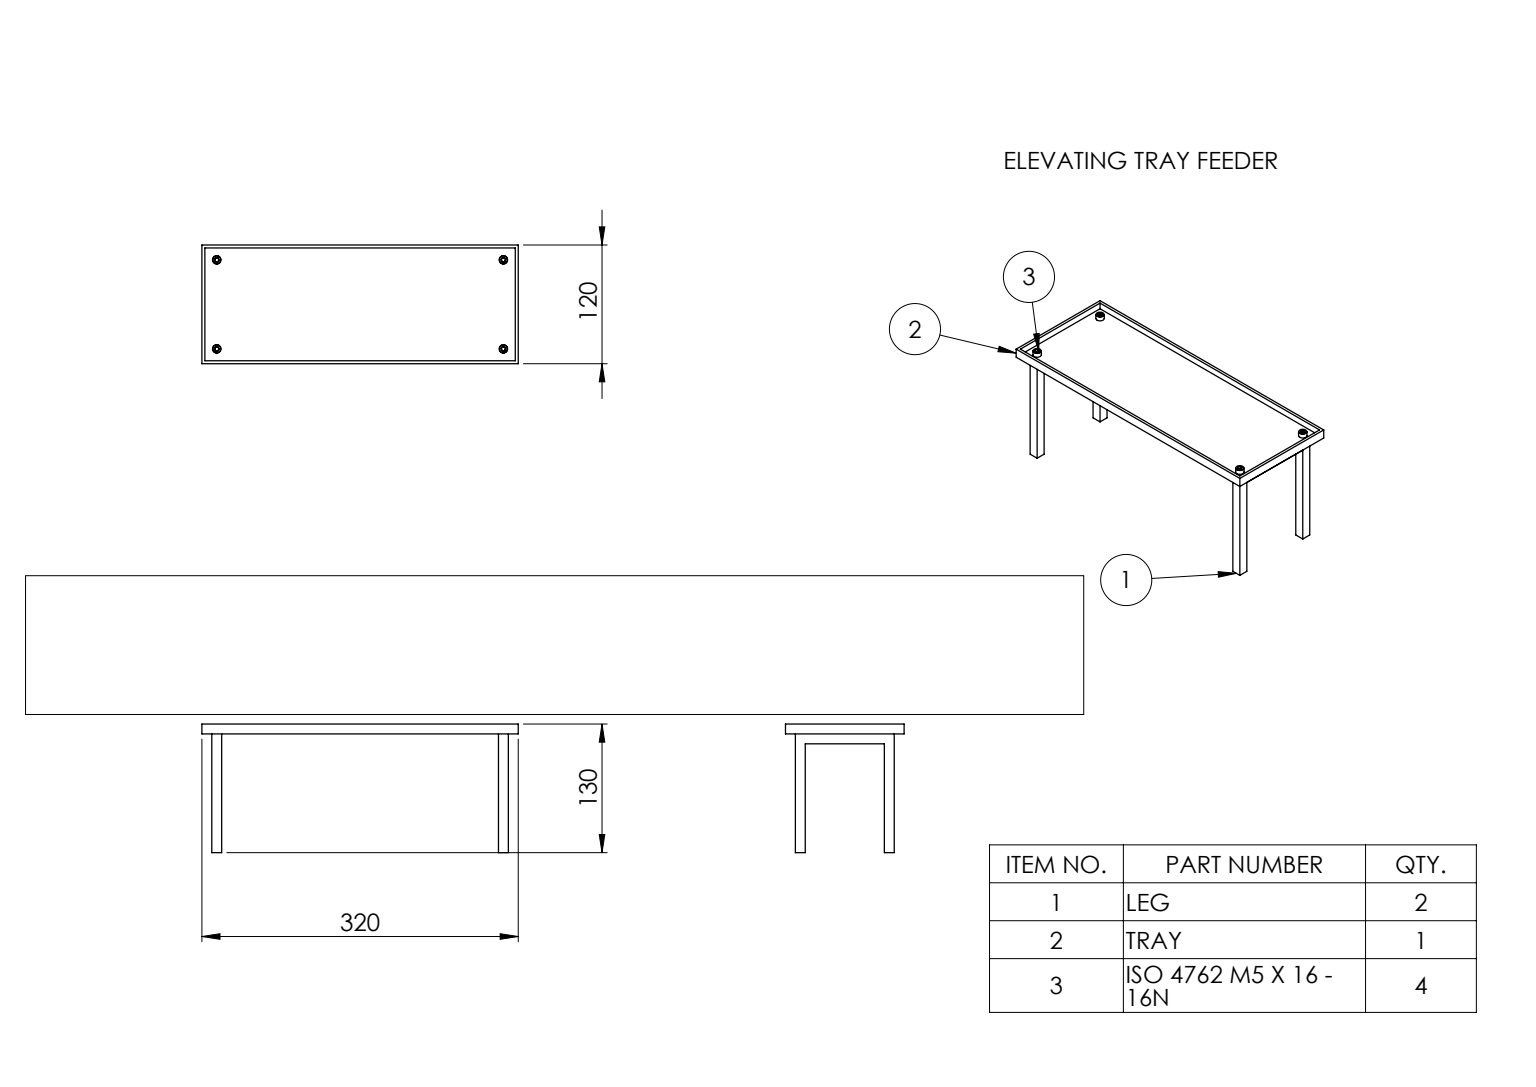
ISO-10303-21;
HEADER;
FILE_DESCRIPTION (('STEP AP214'),
    '1' );
FILE_NAME ('MAS-194',
    '2026-10-23T15:04:32',
    ( '' ),
    ( '' ),
    'SwSTEP 2.0',
    'SolidWorks 2026',
    '' );
FILE_SCHEMA (( 'AUTOMOTIVE_DESIGN' ));
ENDSEC;

DATA;
#1 = AXIS2_PLACEMENT_3D ( 'NONE', #713, #1643, #1457 ) ;
#2 = DIRECTION ( 'NONE',  ( 6.123233995736766036E-17, -1.000000000000000000, 0.000000000000000000 ) ) ;
#3 = AXIS2_PLACEMENT_3D ( 'NONE', #402, #1764, #2101 ) ;
#4 = VERTEX_POINT ( 'NONE', #2115 ) ;
#5 =( REPRESENTATION_RELATIONSHIP ('NONE','NONE', #367, #261 ) REPRESENTATION_RELATIONSHIP_WITH_TRANSFORMATION ( #2142 )SHAPE_REPRESENTATION_RELATIONSHIP( ) );
#6 = ORIENTED_EDGE ( 'NONE', *, *, #567, .F. ) ;
#7 = CARTESIAN_POINT ( 'NONE',  ( 145.0000000000000284, 2.993649167310367343, -47.64999999999998437 ) ) ;
#8 = PLANE ( 'NONE',  #1813 ) ;
#9 = CARTESIAN_POINT ( 'NONE',  ( -145.0000000000000284, -15.00000000000003197, 45.00000000000000000 ) ) ;
#10 = EDGE_CURVE ( 'NONE', #1293, #705, #989, .T. ) ;
#11 = DIRECTION ( 'NONE',  ( 0.000000000000000000, 0.5000000000000009992, 0.8660254037844380415 ) ) ;
#12 = CIRCLE ( 'NONE', #33, 2.500000000000002220 ) ;
#13 = EDGE_CURVE ( 'NONE', #1816, #847, #1494, .T. ) ;
#14 = ORIENTED_EDGE ( 'NONE', *, *, #1898, .T. ) ;
#15 = FACE_OUTER_BOUND ( 'NONE', #510, .T. ) ;
#16 = DIRECTION ( 'NONE',  ( -1.000000000000000000, 0.000000000000000000, 0.000000000000000000 ) ) ;
#17 = DIRECTION ( 'NONE',  ( 1.000000000000000000, 0.000000000000000000, 0.000000000000000000 ) ) ;
#18 = CIRCLE ( 'NONE', #321, 2.700000000000001066 ) ;
#19 = ORIENTED_EDGE ( 'NONE', *, *, #1395, .T. ) ;
#20 = DIRECTION ( 'NONE',  ( 0.000000000000000000, 0.000000000000000000, 1.000000000000000000 ) ) ;
#21 = CARTESIAN_POINT ( 'NONE',  ( 157.0000000000000000, 10.00000000000000000, 3.631354476378115974E-14 ) ) ;
#22 = FILL_AREA_STYLE ('',( #1265 ) ) ;
#23 = VECTOR ( 'NONE', #1974, 1000.000000000000000 ) ;
#24 = ORIENTED_EDGE ( 'NONE', *, *, #1544, .T. ) ;
#25 = CARTESIAN_POINT ( 'NONE',  ( -145.0000000000000284, 3.000000000000000000, -45.00000000000000000 ) ) ;
#26 = DIRECTION ( 'NONE',  ( -0.000000000000000000, 1.000000000000000000, -0.000000000000000000 ) ) ;
#27 = CYLINDRICAL_SURFACE ( 'NONE', #1694, 2.649999999999985700 ) ;
#28 = DIRECTION ( 'NONE',  ( 0.000000000000000000, -0.5000000000000009992, -0.8660254037844380415 ) ) ;
#29 = DIRECTION ( 'NONE',  ( -0.000000000000000000, -0.000000000000000000, -1.000000000000000000 ) ) ;
#30 = AXIS2_PLACEMENT_3D ( 'NONE', #971, #1660, #79 ) ;
#31 = CIRCLE ( 'NONE', #984, 2.649999999999985700 ) ;
#32 = EDGE_LOOP ( 'NONE', ( #1024, #985, #1536, #1885 ) ) ;
#33 = AXIS2_PLACEMENT_3D ( 'NONE', #1749, #1441, #229 ) ;
#34 = VECTOR ( 'NONE', #1991, 1000.000000000000000 ) ;
#35 = ORIENTED_EDGE ( 'NONE', *, *, #686, .F. ) ;
#36 = CYLINDRICAL_SURFACE ( 'NONE', #640, 2.649999999999985700 ) ;
#37 = CARTESIAN_POINT ( 'NONE',  ( 2.500000000000000000, 2.357898499370431722, -2.818925648462311528E-15 ) ) ;
#38 = SHAPE_REPRESENTATION ( 'leg', ( #30 ), #544 ) ;
#39 = DIRECTION ( 'NONE',  ( -6.123233995736766036E-17, 1.000000000000000000, -0.000000000000000000 ) ) ;
#40 = EDGE_CURVE ( 'NONE', #1625, #1348, #636, .T. ) ;
#41 = LINE ( 'NONE', #2054, #907 ) ;
#42 = PRODUCT_RELATED_PRODUCT_CATEGORY ( 'part', '', ( #72 ) ) ;
#43 = CARTESIAN_POINT ( 'NONE',  ( -150.0000000000000000, 0.000000000000000000, 50.00000000000000000 ) ) ;
#44 = VERTEX_POINT ( 'NONE', #1009 ) ;
#45 = ORIENTED_EDGE ( 'NONE', *, *, #1333, .T. ) ;
#46 = CARTESIAN_POINT ( 'NONE',  ( 160.0000000000000000, 0.000000000000000000, -60.00000000000000000 ) ) ;
#47 = CARTESIAN_POINT ( 'NONE',  ( 160.0000000000000000, 10.00000000000000000, -60.00000000000000000 ) ) ;
#48 = PLANE ( 'NONE',  #876 ) ;
#49 = ORIENTED_EDGE ( 'NONE', *, *, #111, .T. ) ;
#50 = DIRECTION ( 'NONE',  ( -0.000000000000000000, 1.000000000000000000, -0.000000000000000000 ) ) ;
#51 = AXIS2_PLACEMENT_3D ( 'NONE', #1269, #57, #1759 ) ;
#52 = CARTESIAN_POINT ( 'NONE',  ( -145.0000000000000284, -15.00000000000003197, -45.00000000000000000 ) ) ;
#53 = EDGE_CURVE ( 'NONE', #738, #333, #1664, .T. ) ;
#54 = ORIENTED_EDGE ( 'NONE', *, *, #1804, .F. ) ;
#55 = EDGE_CURVE ( 'NONE', #1358, #1353, #1429, .T. ) ;
#56 = ORIENTED_EDGE ( 'NONE', *, *, #696, .T. ) ;
#57 = DIRECTION ( 'NONE',  ( 6.123233995736766036E-17, -1.000000000000000000, 0.000000000000000000 ) ) ;
#58 = CARTESIAN_POINT ( 'NONE',  ( 0.000000000000000000, -1.178949249685214307, 2.042000000000001592 ) ) ;
#59 = DIRECTION ( 'NONE',  ( -0.000000000000000000, -1.000000000000000000, -0.000000000000000000 ) ) ;
#60 = VERTEX_POINT ( 'NONE', #817 ) ;
#61 = CIRCLE ( 'NONE', #2078, 2.500000000000002220 ) ;
#62 = DIRECTION ( 'NONE',  ( -0.000000000000000000, 0.000000000000000000, -1.000000000000000000 ) ) ;
#63 = LINE ( 'NONE', #106, #788 ) ;
#64 = ADVANCED_FACE ( 'NONE', ( #2182 ), #1857, .F. ) ;
#65 = VERTEX_POINT ( 'NONE', #648 ) ;
#66 = ADVANCED_FACE ( 'NONE', ( #1330, #2016 ), #1163, .F. ) ;
#67 = AXIS2_PLACEMENT_3D ( 'NONE', #1690, #1835, #1322 ) ;
#68 = ORIENTED_EDGE ( 'NONE', *, *, #53, .F. ) ;
#69 = DIRECTION ( 'NONE',  ( -1.000000000000000000, 0.000000000000000000, -0.000000000000000000 ) ) ;
#70 = LINE ( 'NONE', #2132, #1985 ) ;
#71 = AXIS2_PLACEMENT_3D ( 'NONE', #2013, #995, #1317 ) ;
#72 = PRODUCT ( 'leg', 'leg', '', ( #943 ) ) ;
#74 = ORIENTED_EDGE ( 'NONE', *, *, #1134, .T. ) ;
#73 = CARTESIAN_POINT ( 'NONE',  ( 145.0000000000000284, 2.993649167310367343, -45.00000000000000000 ) ) ;
#75 = CARTESIAN_POINT ( 'NONE',  ( 2.500000000000000000, 1.178949249685212974, -2.042000000000001148 ) ) ;
#76 = DIRECTION ( 'NONE',  ( 0.000000000000000000, 0.000000000000000000, 1.000000000000000000 ) ) ;
#77 = DIRECTION ( 'NONE',  ( 0.000000000000000000, 0.000000000000000000, -1.000000000000000000 ) ) ;
#78 = APPLICATION_PROTOCOL_DEFINITION ( 'draft international standard', 'automotive_design', 1998, #320 ) ;
#79 = DIRECTION ( 'NONE',  ( 1.000000000000000000, 0.000000000000000000, 0.000000000000000000 ) ) ;
#80 = VERTEX_POINT ( 'NONE', #828 ) ;
#81 = ORIENTED_EDGE ( 'NONE', *, *, #373, .T. ) ;
#82 = FACE_OUTER_BOUND ( 'NONE', #1924, .T. ) ;
#83 = FACE_OUTER_BOUND ( 'NONE', #1993, .T. ) ;
#84 = ORIENTED_EDGE ( 'NONE', *, *, #604, .T. ) ;
#86 = ORIENTED_EDGE ( 'NONE', *, *, #306, .T. ) ;
#85 = DIRECTION ( 'NONE',  ( 1.000000000000000000, 0.000000000000000000, 0.000000000000000000 ) ) ;
#87 = FACE_OUTER_BOUND ( 'NONE', #1431, .T. ) ;
#88 = VECTOR ( 'NONE', #539, 1000.000000000000000 ) ;
#89 = DIRECTION ( 'NONE',  ( -0.000000000000000000, 1.000000000000000000, -0.000000000000000000 ) ) ;
#90 = CARTESIAN_POINT ( 'NONE',  ( -157.0000000000000284, 10.00000000000000000, 57.00000000000000711 ) ) ;
#91 = VECTOR ( 'NONE', #730, 1000.000000000000114 ) ;
#92 = APPLICATION_PROTOCOL_DEFINITION ( 'draft international standard', 'automotive_design', 1998, #1085 ) ;
#93 =( LENGTH_UNIT ( ) NAMED_UNIT ( * ) SI_UNIT ( .MILLI., .METRE. ) );
#94 = VERTEX_POINT ( 'NONE', #1687 ) ;
#95 = EDGE_LOOP ( 'NONE', ( #1914, #1029, #1402 ) ) ;
#96 =( LENGTH_UNIT ( ) NAMED_UNIT ( * ) SI_UNIT ( .MILLI., .METRE. ) );
#97 = EDGE_LOOP ( 'NONE', ( #511, #45, #1713, #1611, #2168, #1515, #1183, #1829 ) ) ;
#98 = AXIS2_PLACEMENT_3D ( 'NONE', #2176, #427, #1287 ) ;
#100 = ORIENTED_EDGE ( 'NONE', *, *, #520, .T. ) ;
#99 = DIRECTION ( 'NONE',  ( 0.000000000000000000, 0.000000000000000000, 1.000000000000000000 ) ) ;
#101 = EDGE_CURVE ( 'NONE', #1631, #537, #2026, .T. ) ;
#102 = CARTESIAN_POINT ( 'NONE',  ( -160.0000000000000000, 10.00000000000000000, -56.99999999999997868 ) ) ;
#103 = AXIS2_PLACEMENT_3D ( 'NONE', #1867, #1367, #311 ) ;
#104 = AXIS2_PLACEMENT_3D ( 'NONE', #52, #222, #918 ) ;
#105 = CARTESIAN_POINT ( 'NONE',  ( 2.500000000000000000, 0.000000000000000000, 0.000000000000000000 ) ) ;
#106 = CARTESIAN_POINT ( 'NONE',  ( -139.9999999999999716, 2.312964634635743056E-15, -50.00000000000000000 ) ) ;
#107 = APPLICATION_PROTOCOL_DEFINITION ( 'draft international standard', 'automotive_design', 1998, #888 ) ;
#108 = ORIENTED_EDGE ( 'NONE', *, *, #1169, .T. ) ;
#109 = PLANE ( 'NONE',  #1726 ) ;
#110 = ORIENTED_EDGE ( 'NONE', *, *, #318, .F. ) ;
#111 = EDGE_CURVE ( 'NONE', #1963, #60, #1752, .T. ) ;
#112 = CARTESIAN_POINT ( 'NONE',  ( -139.9999999999999716, 2.312964634635743056E-15, 50.00000000000000000 ) ) ;
#113 = AXIS2_PLACEMENT_3D ( 'NONE', #174, #1044, #1337 ) ;
#114 = DIRECTION ( 'NONE',  ( 1.000000000000000000, 0.000000000000000000, -4.336808689942017736E-17 ) ) ;
#115 = ADVANCED_FACE ( 'NONE', ( #2005 ), #793, .T. ) ;
#116 = ADVANCED_FACE ( 'NONE', ( #1527 ), #1518, .T. ) ;
#117 =( GEOMETRIC_REPRESENTATION_CONTEXT ( 3 ) GLOBAL_UNCERTAINTY_ASSIGNED_CONTEXT ( ( #842 ) ) GLOBAL_UNIT_ASSIGNED_CONTEXT ( ( #1606, #589, #1445 ) ) REPRESENTATION_CONTEXT ( 'NONE', 'WORKASPACE' ) );
#118 = PRODUCT ( 'MAS-194', 'MAS-194', '', ( #1624 ) ) ;
#119 = CARTESIAN_POINT ( 'NONE',  ( -145.0000000000000284, 0.000000000000000000, 42.35000000000001563 ) ) ;
#120 = CARTESIAN_POINT ( 'NONE',  ( 156.9999999999999716, 3.000000000000000000, 57.00000000000000711 ) ) ;
#121 = EDGE_CURVE ( 'NONE', #1963, #166, #205, .T. ) ;
#122 = SHAPE_DEFINITION_REPRESENTATION ( #806, #367 ) ;
#123 = ORIENTED_EDGE ( 'NONE', *, *, #401, .T. ) ;
#124 = LINE ( 'NONE', #1842, #1158 ) ;
#125 = ORIENTED_EDGE ( 'NONE', *, *, #416, .T. ) ;
#126 = CARTESIAN_POINT ( 'NONE',  ( 21.00000000000000355, 0.000000000000000000, 0.000000000000000000 ) ) ;
#127 = LINE ( 'NONE', #2039, #1839 ) ;
#128 = DIRECTION ( 'NONE',  ( 1.000000000000000000, 0.000000000000000000, 0.000000000000000000 ) ) ;
#129 = AXIS2_PLACEMENT_3D ( 'NONE', #1889, #358, #1728 ) ;
#130 = DIRECTION ( 'NONE',  ( 0.000000000000000000, -1.000000000000000000, 0.000000000000000000 ) ) ;
#131 = FILL_AREA_STYLE_COLOUR ( '', #721 ) ;
#132 = ADVANCED_FACE ( 'NONE', ( #2209 ), #2220, .F. ) ;
#133 = ORIENTED_EDGE ( 'NONE', *, *, #586, .T. ) ;
#134 = DIRECTION ( 'NONE',  ( 2.312964634635742957E-16, -1.000000000000000000, 0.000000000000000000 ) ) ;
#135 = EDGE_CURVE ( 'NONE', #1670, #1316, #2046, .T. ) ;
#136 = ORIENTED_EDGE ( 'NONE', *, *, #518, .T. ) ;
#137 = CARTESIAN_POINT ( 'NONE',  ( 145.0000000000000284, 3.000000000000002665, -45.00000000000000000 ) ) ;
#138 = DIRECTION ( 'NONE',  ( 1.000000000000000000, 0.000000000000000000, 0.000000000000000000 ) ) ;
#139 = CIRCLE ( 'NONE', #605, 2.500000000000000444 ) ;
#140 = EDGE_LOOP ( 'NONE', ( #2012, #1805, #2066, #1757, #813 ) ) ;
#141 = DIRECTION ( 'NONE',  ( 0.000000000000000000, 0.000000000000000000, -1.000000000000000000 ) ) ;
#142 = DIRECTION ( 'NONE',  ( 0.000000000000000000, 0.000000000000000000, -1.000000000000000000 ) ) ;
#143 = SURFACE_SIDE_STYLE ('',( #858 ) ) ;
#144 = EDGE_CURVE ( 'NONE', #1505, #145, #1507, .T. ) ;
#145 = VERTEX_POINT ( 'NONE', #489 ) ;
#146 = ADVANCED_FACE ( 'NONE', ( #978 ), #2193, .F. ) ;
#147 = DIRECTION ( 'NONE',  ( -1.000000000000000000, 0.000000000000000000, -0.000000000000000000 ) ) ;
#148 = ORIENTED_EDGE ( 'NONE', *, *, #1970, .F. ) ;
#149 = CARTESIAN_POINT ( 'NONE',  ( 0.2500000000000002220, 0.000000000000000000, 0.000000000000000000 ) ) ;
#150 = CARTESIAN_POINT ( 'NONE',  ( 2.500000000000000000, 2.357898499370431722, -2.818925648462311528E-15 ) ) ;
#151 = ORIENTED_EDGE ( 'NONE', *, *, #1176, .T. ) ;
#152 = VECTOR ( 'NONE', #723, 1000.000000000000000 ) ;
#153 = DIRECTION ( 'NONE',  ( 0.000000000000000000, -1.000000000000000000, 0.000000000000000000 ) ) ;
#154 = FACE_OUTER_BOUND ( 'NONE', #1037, .T. ) ;
#155 = AXIS2_PLACEMENT_3D ( 'NONE', #797, #1356, #500 ) ;
#156 = AXIS2_PLACEMENT_3D ( 'NONE', #1101, #1761, #935 ) ;
#157 = ORIENTED_EDGE ( 'NONE', *, *, #401, .F. ) ;
#158 = ORIENTED_EDGE ( 'NONE', *, *, #281, .T. ) ;
#159 = DIRECTION ( 'NONE',  ( 0.000000000000000000, -1.000000000000000000, 0.000000000000000000 ) ) ;
#160 = CARTESIAN_POINT ( 'NONE',  ( -145.0000000000000284, 3.000000000000001776, -47.70000000000000284 ) ) ;
#161 = UNCERTAINTY_MEASURE_WITH_UNIT (LENGTH_MEASURE( 1.000000000000000082E-05 ), #96, 'distance_accuracy_value', 'NONE');
#162 = EDGE_LOOP ( 'NONE', ( #1939, #248, #188, #677 ) ) ;
#163 = CARTESIAN_POINT ( 'NONE',  ( -31.74999999999995737, 0.000000000000000000, 0.000000000000000000 ) ) ;
#164 = CARTESIAN_POINT ( 'NONE',  ( 5.200000000000002842, 0.000000000000000000, 2.500000000000000444 ) ) ;
#165 = EDGE_CURVE ( 'NONE', #314, #2053, #1896, .T. ) ;
#166 = VERTEX_POINT ( 'NONE', #1403 ) ;
#167 = ORIENTED_EDGE ( 'NONE', *, *, #1762, .T. ) ;
#168 = VECTOR ( 'NONE', #1538, 1000.000000000000000 ) ;
#169 = CYLINDRICAL_SURFACE ( 'NONE', #1242, 2.649999999999985700 ) ;
#170 = CARTESIAN_POINT ( 'NONE',  ( -157.0000000000000000, 10.00000000000000000, -3.631354476378115974E-14 ) ) ;
#171 = ADVANCED_FACE ( 'NONE', ( #512 ), #704, .T. ) ;
#172 = EDGE_LOOP ( 'NONE', ( #1456, #1524 ) ) ;
#173 = DIRECTION ( 'NONE',  ( -1.000000000000000000, 0.000000000000000000, 0.000000000000000000 ) ) ;
#174 = CARTESIAN_POINT ( 'NONE',  ( 0.000000000000000000, 0.000000000000000000, 0.000000000000000000 ) ) ;
#175 = CLOSED_SHELL ( 'NONE', ( #313, #917, #64, #1213, #1876, #1890, #1705, #1823, #1721, #1503, #2061, #116, #1440, #2153, #1530, #1941, #1489, #1042 ) ) ;
#176 = ORIENTED_EDGE ( 'NONE', *, *, #1772, .T. ) ;
#177 = AXIS2_PLACEMENT_3D ( 'NONE', #1608, #438, #449 ) ;
#178 = ORIENTED_EDGE ( 'NONE', *, *, #684, .F. ) ;
#179 = FACE_OUTER_BOUND ( 'NONE', #272, .T. ) ;
#180 = EDGE_CURVE ( 'NONE', #226, #627, #965, .T. ) ;
#181 = CARTESIAN_POINT ( 'NONE',  ( -160.0000000000000284, 0.000000000000000000, 60.00000000000001421 ) ) ;
#182 = AXIS2_PLACEMENT_3D ( 'NONE', #632, #455, #1006 ) ;
#183 = AXIS2_PLACEMENT_3D ( 'NONE', #2092, #526, #1052 ) ;
#184 = ADVANCED_FACE ( 'NONE', ( #1232 ), #388, .T. ) ;
#185 = DIRECTION ( 'NONE',  ( 0.000000000000000000, 0.000000000000000000, -1.000000000000000000 ) ) ;
#186 = EDGE_CURVE ( 'NONE', #1465, #166, #1054, .T. ) ;
#187 = AXIS2_PLACEMENT_3D ( 'NONE', #646, #1683, #147 ) ;
#188 = ORIENTED_EDGE ( 'NONE', *, *, #880, .T. ) ;
#189 = CARTESIAN_POINT ( 'NONE',  ( 5.200000000000002842, 0.000000000000000000, 0.000000000000000000 ) ) ;
#190 = DIRECTION ( 'NONE',  ( 0.000000000000000000, -0.4999999999999989453, 0.8660254037844391517 ) ) ;
#191 = CARTESIAN_POINT ( 'NONE',  ( -145.0000000000000284, -15.00000000000003197, 47.50000000000000000 ) ) ;
#192 = DIRECTION ( 'NONE',  ( -1.000000000000000000, -0.000000000000000000, -0.000000000000000000 ) ) ;
#193 = LINE ( 'NONE', #908, #1216 ) ;
#194 = CIRCLE ( 'NONE', #1276, 2.500000000000002220 ) ;
#195 = ORIENTED_EDGE ( 'NONE', *, *, #283, .T. ) ;
#196 = CARTESIAN_POINT ( 'NONE',  ( 2.500000000000000000, 1.178949249685212974, -2.042000000000001148 ) ) ;
#197 = EDGE_CURVE ( 'NONE', #1465, #610, #889, .T. ) ;
#198 = DIRECTION ( 'NONE',  ( -0.000000000000000000, 1.000000000000000000, -0.000000000000000000 ) ) ;
#199 = LINE ( 'NONE', #1861, #548 ) ;
#200 = CARTESIAN_POINT ( 'NONE',  ( 5.200000000000002842, 0.000000000000000000, 0.000000000000000000 ) ) ;
#201 = DIRECTION ( 'NONE',  ( -1.000000000000000000, -0.000000000000000000, -0.000000000000000000 ) ) ;
#202 = CARTESIAN_POINT ( 'NONE',  ( 145.0000000000000284, 3.000000000000001776, -47.70000000000000284 ) ) ;
#203 = AXIS2_PLACEMENT_3D ( 'NONE', #709, #130, #651 ) ;
#204 = ORIENTED_EDGE ( 'NONE', *, *, #1315, .F. ) ;
#205 = CIRCLE ( 'NONE', #1463, 2.649999999999985700 ) ;
#206 = ORIENTED_EDGE ( 'NONE', *, *, #1935, .T. ) ;
#207 = DIRECTION ( 'NONE',  ( 1.000000000000000000, 0.000000000000000000, 0.000000000000000000 ) ) ;
#208 = EDGE_CURVE ( 'NONE', #749, #899, #1717, .T. ) ;
#209 = DIRECTION ( 'NONE',  ( 0.000000000000000000, 0.000000000000000000, -1.000000000000000000 ) ) ;
#210 = CARTESIAN_POINT ( 'NONE',  ( -160.0000000000000000, 10.00000000000000000, -59.99999999999998579 ) ) ;
#211 = DIRECTION ( 'NONE',  ( 0.000000000000000000, 0.000000000000000000, -1.000000000000000000 ) ) ;
#212 = CARTESIAN_POINT ( 'NONE',  ( 2.500000000000000000, -2.357898499370432166, 3.035766082959412415E-15 ) ) ;
#213 = PRESENTATION_LAYER_ASSIGNMENT (  '', '', ( #1119 ) ) ;
#214 = EDGE_LOOP ( 'NONE', ( #762, #945, #1306, #1209 ) ) ;
#215 = PRESENTATION_LAYER_ASSIGNMENT (  '', '', ( #341 ) ) ;
#216 = VERTEX_POINT ( 'NONE', #7 ) ;
#217 = FACE_OUTER_BOUND ( 'NONE', #1185, .T. ) ;
#218 = CARTESIAN_POINT ( 'NONE',  ( 160.0000000000000000, 10.00000000000000000, -60.00000000000000000 ) ) ;
#219 = DIRECTION ( 'NONE',  ( 4.336808689942017736E-17, -0.000000000000000000, 1.000000000000000000 ) ) ;
#220 = VERTEX_POINT ( 'NONE', #2089 ) ;
#221 = FILL_AREA_STYLE_COLOUR ( '', #1658 ) ;
#222 = DIRECTION ( 'NONE',  ( -0.000000000000000000, 1.000000000000000000, -0.000000000000000000 ) ) ;
#223 = DIRECTION ( 'NONE',  ( -1.000000000000000000, -6.123233995736766036E-17, -0.000000000000000000 ) ) ;
#224 = EDGE_CURVE ( 'NONE', #575, #1831, #600, .T. ) ;
#225 = ORIENTED_EDGE ( 'NONE', *, *, #1492, .F. ) ;
#226 = VERTEX_POINT ( 'NONE', #357 ) ;
#227 = CIRCLE ( 'NONE', #385, 2.700000000000001066 ) ;
#228 = LINE ( 'NONE', #585, #1036 ) ;
#229 = DIRECTION ( 'NONE',  ( 0.000000000000000000, 0.000000000000000000, 1.000000000000000000 ) ) ;
#230 = CARTESIAN_POINT ( 'NONE',  ( -160.0000000000000284, 10.00000000000000000, 60.00000000000001421 ) ) ;
#231 = CARTESIAN_POINT ( 'NONE',  ( -2.471980953266949321E-15, 3.000000000000000000, -56.99999999999998579 ) ) ;
#232 = EDGE_CURVE ( 'NONE', #65, #2053, #1572, .T. ) ;
#233 = CIRCLE ( 'NONE', #866, 4.250000000000000000 ) ;
#234 = ORIENTED_EDGE ( 'NONE', *, *, #1075, .T. ) ;
#235 = ORIENTED_EDGE ( 'NONE', *, *, #197, .F. ) ;
#236 = CARTESIAN_POINT ( 'NONE',  ( 3.678949249685231848, 0.000000000000000000, 0.000000000000000000 ) ) ;
#237 = DIRECTION ( 'NONE',  ( -0.000000000000000000, -0.000000000000000000, -1.000000000000000000 ) ) ;
#238 = FACE_OUTER_BOUND ( 'NONE', #1600, .T. ) ;
#240 = VERTEX_POINT ( 'NONE', #1377 ) ;
#239 = CARTESIAN_POINT ( 'NONE',  ( 2.500000000000000000, 2.357898499370431722, -2.818925648462311528E-15 ) ) ;
#241 = PRESENTATION_STYLE_ASSIGNMENT (( #2112 ) ) ;
#242 = AXIS2_PLACEMENT_3D ( 'NONE', #919, #223, #2104 ) ;
#243 = DIRECTION ( 'NONE',  ( -1.000000000000000000, 0.000000000000000000, 4.336808689942017736E-17 ) ) ;
#244 = DIRECTION ( 'NONE',  ( -5.046468293750711010E-16, 1.000000000000000000, 0.000000000000000000 ) ) ;
#245 = CONTEXT_DEPENDENT_SHAPE_REPRESENTATION ( #1913, #2164 ) ;
#246 = ADVANCED_FACE ( 'NONE', ( #1385 ), #1674, .T. ) ;
#247 =( LENGTH_UNIT ( ) NAMED_UNIT ( * ) SI_UNIT ( .MILLI., .METRE. ) );
#248 = ORIENTED_EDGE ( 'NONE', *, *, #706, .T. ) ;
#249 = ORIENTED_EDGE ( 'NONE', *, *, #424, .F. ) ;
#250 = VECTOR ( 'NONE', #1166, 1000.000000000000000 ) ;
#251 = ORIENTED_EDGE ( 'NONE', *, *, #1272, .F. ) ;
#252 = DIRECTION ( 'NONE',  ( -0.000000000000000000, 1.000000000000000000, -0.000000000000000000 ) ) ;
#253 = CARTESIAN_POINT ( 'NONE',  ( -145.0000000000000284, 3.000000000000002665, 45.00000000000000000 ) ) ;
#254 = CIRCLE ( 'NONE', #3, 4.000000000000000000 ) ;
#255 = VECTOR ( 'NONE', #2191, 1000.000000000000000 ) ;
#256 = VERTEX_POINT ( 'NONE', #1555 ) ;
#257 = PRODUCT_DEFINITION_SHAPE ( 'NONE', 'NONE',  #2227 ) ;
#259 = ORIENTED_EDGE ( 'NONE', *, *, #781, .F. ) ;
#258 = DIRECTION ( 'NONE',  ( -0.000000000000000000, 1.000000000000000000, -0.000000000000000000 ) ) ;
#260 = DIRECTION ( 'NONE',  ( -1.000000000000000000, -6.123233995736766036E-17, -0.000000000000000000 ) ) ;
#261 = SHAPE_REPRESENTATION ( 'tray', ( #30 ), #1049 ) ;
#262 = DIRECTION ( 'NONE',  ( 0.000000000000000000, -1.000000000000000000, 0.000000000000000000 ) ) ;
#263 = LINE ( 'NONE', #90, #1184 ) ;
#264 = SURFACE_STYLE_USAGE ( .BOTH. , #1999 ) ;
#265 = ORIENTED_EDGE ( 'NONE', *, *, #1150, .F. ) ;
#266 = EDGE_CURVE ( 'NONE', #1421, #653, #1916, .T. ) ;
#267 = VERTEX_POINT ( 'NONE', #707 ) ;
#268 = DIRECTION ( 'NONE',  ( 0.000000000000000000, 0.000000000000000000, -1.000000000000000000 ) ) ;
#269 = CARTESIAN_POINT ( 'NONE',  ( -150.0000000000000000, 0.000000000000000000, -50.00000000000000000 ) ) ;
#270 = EDGE_LOOP ( 'NONE', ( #655, #206, #1374 ) ) ;
#272 = EDGE_LOOP ( 'NONE', ( #1135, #854, #1328, #1129 ) ) ;
#271 = LINE ( 'NONE', #1566, #1453 ) ;
#273 = CARTESIAN_POINT ( 'NONE',  ( 145.0000000000000284, 2.800000000000000266, -45.00000000000000000 ) ) ;
#274 = AXIS2_PLACEMENT_3D ( 'NONE', #873, #679, #190 ) ;
#275 = CARTESIAN_POINT ( 'NONE',  ( 0.000000000000000000, 0.000000000000000000, 50.00000000000000000 ) ) ;
#276 = FACE_OUTER_BOUND ( 'NONE', #1110, .T. ) ;
#277 = AXIS2_PLACEMENT_3D ( 'NONE', #538, #1561, #1211 ) ;
#278 = DIRECTION ( 'NONE',  ( 1.000000000000000000, 0.000000000000000000, 0.000000000000000000 ) ) ;
#279 = PRODUCT_DEFINITION_SHAPE ( 'NONE', 'NONE',  #1642 ) ;
#280 = ORIENTED_EDGE ( 'NONE', *, *, #988, .T. ) ;
#281 = EDGE_CURVE ( 'NONE', #240, #1735, #1638, .T. ) ;
#282 = ORIENTED_EDGE ( 'NONE', *, *, #559, .F. ) ;
#283 = EDGE_CURVE ( 'NONE', #1794, #1470, #1533, .T. ) ;
#284 = CARTESIAN_POINT ( 'NONE',  ( -145.0000000000000284, -15.00000000000003197, 42.49999999999999289 ) ) ;
#285 = ORIENTED_EDGE ( 'NONE', *, *, #1767, .T. ) ;
#286 = AXIS2_PLACEMENT_3D ( 'NONE', #1522, #857, #1497 ) ;
#287 = ADVANCED_FACE ( 'NONE', ( #15 ), #36, .F. ) ;
#288 = DIRECTION ( 'NONE',  ( 0.000000000000000000, -0.5000000000000013323, -0.8660254037844380415 ) ) ;
#289 = DIRECTION ( 'NONE',  ( 0.000000000000000000, 0.000000000000000000, 1.000000000000000000 ) ) ;
#290 = CLOSED_SHELL ( 'NONE', ( #1208, #1730, #801, #1062, #184, #534, #1347, #1500, #1560, #469, #1546, #374, #979, #115, #1267, #2103, #1607, #1259, #869, #1380, #531, #1775, #1016, #132, #451, #1373, #1562 ) ) ;
#291 = COLOUR_RGB ( '',0.8941176470588234615, 0.8941176470588234615, 0.8941176470588234615 ) ;
#292 = CARTESIAN_POINT ( 'NONE',  ( 0.000000000000000000, -2.357898499370432166, 3.035766082959412415E-15 ) ) ;
#293 = CARTESIAN_POINT ( 'NONE',  ( 2.500000000000000000, 1.178949249685217415, 2.041999999999998483 ) ) ;
#294 = ORIENTED_EDGE ( 'NONE', *, *, #359, .T. ) ;
#295 = DIRECTION ( 'NONE',  ( 0.000000000000000000, -0.5000000000000009992, -0.8660254037844380415 ) ) ;
#296 = ORIENTED_EDGE ( 'NONE', *, *, #1610, .F. ) ;
#297 =( GEOMETRIC_REPRESENTATION_CONTEXT ( 3 ) GLOBAL_UNCERTAINTY_ASSIGNED_CONTEXT ( ( #1869 ) ) GLOBAL_UNIT_ASSIGNED_CONTEXT ( ( #1381, #1558, #1182 ) ) REPRESENTATION_CONTEXT ( 'NONE', 'WORKASPACE' ) );
#298 = AXIS2_PLACEMENT_3D ( 'NONE', #2174, #1189, #2020 ) ;
#299 = DIRECTION ( 'NONE',  ( 0.000000000000000000, 0.5150380749100541555, 0.8571673007021122226 ) ) ;
#300 = AXIS2_PLACEMENT_3D ( 'NONE', #508, #495, #1703 ) ;
#301 = CARTESIAN_POINT ( 'NONE',  ( 2.500000000000000000, 0.000000000000000000, 0.000000000000000000 ) ) ;
#302 = AXIS2_PLACEMENT_3D ( 'NONE', #75, #1797, #1080 ) ;
#303 = CARTESIAN_POINT ( 'NONE',  ( 2.500000000000000000, 1.178949249685212974, -2.042000000000001148 ) ) ;
#304 = DIRECTION ( 'NONE',  ( -1.000000000000000000, -0.000000000000000000, -0.000000000000000000 ) ) ;
#305 = ADVANCED_FACE ( 'NONE', ( #1736 ), #169, .F. ) ;
#306 = EDGE_CURVE ( 'NONE', #4, #1672, #1360, .T. ) ;
#307 =( NAMED_UNIT ( * ) PLANE_ANGLE_UNIT ( ) SI_UNIT ( $, .RADIAN. ) );
#308 = ORIENTED_EDGE ( 'NONE', *, *, #734, .F. ) ;
#309 = CARTESIAN_POINT ( 'NONE',  ( -139.9999999999999716, -120.0000000000000142, 40.00000000000000000 ) ) ;
#310 = ORIENTED_EDGE ( 'NONE', *, *, #2133, .T. ) ;
#311 = DIRECTION ( 'NONE',  ( 0.000000000000000000, -1.000000000000000000, 0.000000000000000000 ) ) ;
#312 = CARTESIAN_POINT ( 'NONE',  ( 0.000000000000000000, 0.000000000000000000, 0.000000000000000000 ) ) ;
#313 = ADVANCED_FACE ( 'NONE', ( #1926 ), #1245, .F. ) ;
#314 = VERTEX_POINT ( 'NONE', #236 ) ;
#315 = DIRECTION ( 'NONE',  ( -6.123233995736766036E-17, 1.000000000000000000, -0.000000000000000000 ) ) ;
#316 = CIRCLE ( 'NONE', #1206, 2.500000000000000888 ) ;
#317 = CARTESIAN_POINT ( 'NONE',  ( -145.0000000000000284, 0.000000000000000000, -45.00000000000000000 ) ) ;
#318 = EDGE_CURVE ( 'NONE', #2053, #1816, #228, .T. ) ;
#319 = PRESENTATION_STYLE_ASSIGNMENT (( #1548 ) ) ;
#320 = APPLICATION_CONTEXT ( 'automotive_design' ) ;
#321 = AXIS2_PLACEMENT_3D ( 'NONE', #1424, #399, #1951 ) ;
#322 = ORIENTED_EDGE ( 'NONE', *, *, #1708, .F. ) ;
#323 = DIRECTION ( 'NONE',  ( -0.000000000000000000, 1.000000000000000000, -0.000000000000000000 ) ) ;
#324 = VERTEX_POINT ( 'NONE', #2098 ) ;
#325 = DIRECTION ( 'NONE',  ( -1.000000000000000000, -0.000000000000000000, -0.000000000000000000 ) ) ;
#326 = DIRECTION ( 'NONE',  ( 6.123233995736766036E-17, -1.000000000000000000, 0.000000000000000000 ) ) ;
#327 = AXIS2_PLACEMENT_3D ( 'NONE', #1511, #1026, #1679 ) ;
#328 = ORIENTED_EDGE ( 'NONE', *, *, #868, .F. ) ;
#329 = FACE_OUTER_BOUND ( 'NONE', #1684, .T. ) ;
#330 = DIRECTION ( 'NONE',  ( 2.312964634635742957E-16, 0.000000000000000000, -1.000000000000000000 ) ) ;
#331 = DIRECTION ( 'NONE',  ( 0.000000000000000000, 0.000000000000000000, 1.000000000000000000 ) ) ;
#332 = ORIENTED_EDGE ( 'NONE', *, *, #1547, .T. ) ;
#333 = VERTEX_POINT ( 'NONE', #561 ) ;
#334 = EDGE_CURVE ( 'NONE', #396, #60, #18, .T. ) ;
#335 = CARTESIAN_POINT ( 'NONE',  ( -139.9999999999999716, -120.0000000000000142, 40.00000000000000000 ) ) ;
#336 = MECHANICAL_DESIGN_GEOMETRIC_PRESENTATION_REPRESENTATION (  '', ( #1119 ), #1476 ) ;
#337 = ORIENTED_EDGE ( 'NONE', *, *, #2208, .F. ) ;
#338 = VECTOR ( 'NONE', #28, 1000.000000000000114 ) ;
#339 = CARTESIAN_POINT ( 'NONE',  ( -157.0000000000000284, 3.000000000000000000, 57.00000000000000711 ) ) ;
#340 = DIRECTION ( 'NONE',  ( -2.312964634635743450E-16, 1.000000000000000000, 0.000000000000000000 ) ) ;
#341=STYLED_ITEM('',(#2247),#969);
#342 = DIRECTION ( 'NONE',  ( -1.000000000000000000, 0.000000000000000000, 0.000000000000000000 ) ) ;
#343 = EDGE_LOOP ( 'NONE', ( #996, #736, #151, #176 ) ) ;
#344 = VERTEX_POINT ( 'NONE', #572 ) ;
#345 = ADVANCED_FACE ( 'NONE', ( #1256 ), #564, .T. ) ;
#346 = DIRECTION ( 'NONE',  ( 0.000000000000000000, 0.000000000000000000, 1.000000000000000000 ) ) ;
#347 = CARTESIAN_POINT ( 'NONE',  ( -139.9999999999999716, -120.0000000000000142, -40.00000000000000000 ) ) ;
#348 = UNCERTAINTY_MEASURE_WITH_UNIT (LENGTH_MEASURE( 1.000000000000000082E-05 ), #93, 'distance_accuracy_value', 'NONE');
#349 = EDGE_LOOP ( 'NONE', ( #249, #593, #1950, #1766 ) ) ;
#350 = DIRECTION ( 'NONE',  ( 1.000000000000000000, 0.000000000000000000, 0.000000000000000000 ) ) ;
#351 = EDGE_LOOP ( 'NONE', ( #436, #2147 ) ) ;
#352 = ADVANCED_FACE ( 'NONE', ( #217 ), #1742, .T. ) ;
#353 = VERTEX_POINT ( 'NONE', #46 ) ;
#354 = SHAPE_REPRESENTATION ( 'socket head cap screw_iso_ISO 4762 M5 x 16 - 16N', ( #30 ), #1018 ) ;
#355 = AXIS2_PLACEMENT_3D ( 'NONE', #1066, #872, #1906 ) ;
#356 = EDGE_CURVE ( 'NONE', #705, #671, #1769, .T. ) ;
#357 = CARTESIAN_POINT ( 'NONE',  ( 5.000000000000002665, 0.000000000000000000, -2.700000000000000622 ) ) ;
#358 = DIRECTION ( 'NONE',  ( 6.123233995736766036E-17, -1.000000000000000000, 0.000000000000000000 ) ) ;
#359 = EDGE_CURVE ( 'NONE', #738, #1430, #1432, .T. ) ;
#360 = CARTESIAN_POINT ( 'NONE',  ( 2.500000000000000000, 1.768423874527822459, -1.021000000000002794 ) ) ;
#361 = COLOUR_RGB ( '',1.000000000000000000, 0.9490196078431372140, 0.9098039215686274384 ) ;
#362 = CARTESIAN_POINT ( 'NONE',  ( 0.000000000000000000, 0.000000000000000000, 0.000000000000000000 ) ) ;
#363 = PRESENTATION_LAYER_ASSIGNMENT (  '', '', ( #1329 ) ) ;
#364 = ORIENTED_EDGE ( 'NONE', *, *, #1034, .F. ) ;
#365 = DIRECTION ( 'NONE',  ( 0.000000000000000000, 0.000000000000000000, -1.000000000000000000 ) ) ;
#366 = CARTESIAN_POINT ( 'NONE',  ( -145.0000000000000284, -16.50215154756893554, 45.00000000000000000 ) ) ;
#367 = SHAPE_REPRESENTATION ( 'MAS-194', ( #1338, #691, #113, #1944, #1262, #300, #874, #369 ), #476 ) ;
#368 = FACE_OUTER_BOUND ( 'NONE', #1880, .T. ) ;
#369 = AXIS2_PLACEMENT_3D ( 'NONE', #1523, #2216, #1191 ) ;
#370 = VECTOR ( 'NONE', #446, 1000.000000000000000 ) ;
#371 = DIRECTION ( 'NONE',  ( 0.000000000000000000, -0.5000000000000013323, -0.8660254037844380415 ) ) ;
#372 = VECTOR ( 'NONE', #803, 1000.000000000000000 ) ;
#373 = EDGE_CURVE ( 'NONE', #1909, #1887, #2134, .T. ) ;
#374 = ADVANCED_FACE ( 'NONE', ( #1128 ), #1994, .T. ) ;
#375 = EDGE_LOOP ( 'NONE', ( #1502, #922, #259, #2033 ) ) ;
#376 = LINE ( 'NONE', #347, #1059 ) ;
#377 = DIRECTION ( 'NONE',  ( 0.000000000000000000, -1.000000000000000000, 0.000000000000000000 ) ) ;
#378 = EDGE_CURVE ( 'NONE', #220, #830, #1795, .T. ) ;
#379 = EDGE_LOOP ( 'NONE', ( #1466, #491 ) ) ;
#380 = LINE ( 'NONE', #554, #722 ) ;
#381 = EDGE_CURVE ( 'NONE', #344, #473, #457, .T. ) ;
#382 = DIRECTION ( 'NONE',  ( 1.000000000000000000, 0.000000000000000000, 0.000000000000000000 ) ) ;
#383 = DIRECTION ( 'NONE',  ( -0.000000000000000000, 1.000000000000000000, -0.000000000000000000 ) ) ;
#384 = EDGE_CURVE ( 'NONE', #463, #1794, #597, .T. ) ;
#385 = AXIS2_PLACEMENT_3D ( 'NONE', #1320, #1495, #1483 ) ;
#386 = ORIENTED_EDGE ( 'NONE', *, *, #744, .T. ) ;
#387 = ORIENTED_EDGE ( 'NONE', *, *, #767, .F. ) ;
#388 = CYLINDRICAL_SURFACE ( 'NONE', #1179, 2.500000000000000444 ) ;
#389 = CYLINDRICAL_SURFACE ( 'NONE', #1669, 2.649999999999985700 ) ;
#390 = PLANE ( 'NONE',  #760 ) ;
#391 = AXIS2_PLACEMENT_3D ( 'NONE', #2068, #2060, #524 ) ;
#392 = CARTESIAN_POINT ( 'NONE',  ( -160.0000000000000284, 10.00000000000000000, 60.00000000000001421 ) ) ;
#393 = FACE_OUTER_BOUND ( 'NONE', #1768, .T. ) ;
#394 = SURFACE_STYLE_USAGE ( .BOTH. , #2095 ) ;
#395 = AXIS2_PLACEMENT_3D ( 'NONE', #1475, #639, #1634 ) ;
#396 = VERTEX_POINT ( 'NONE', #2094 ) ;
#397 = VECTOR ( 'NONE', #1100, 1000.000000000000000 ) ;
#398 = EDGE_LOOP ( 'NONE', ( #310, #2160, #521, #2213 ) ) ;
#399 = DIRECTION ( 'NONE',  ( -6.123233995736766036E-17, 1.000000000000000000, -0.000000000000000000 ) ) ;
#400 = FACE_OUTER_BOUND ( 'NONE', #1537, .T. ) ;
#401 = EDGE_CURVE ( 'NONE', #314, #575, #271, .T. ) ;
#402 = CARTESIAN_POINT ( 'NONE',  ( 0.000000000000000000, 0.000000000000000000, 0.000000000000000000 ) ) ;
#403 = DIRECTION ( 'NONE',  ( 0.000000000000000000, 0.000000000000000000, 1.000000000000000000 ) ) ;
#404 = COLOUR_RGB ( '',0.8941176470588234615, 0.8941176470588234615, 0.8941176470588234615 ) ;
#405 = VERTEX_POINT ( 'NONE', #555 ) ;
#406 = AXIS2_PLACEMENT_3D ( 'NONE', #490, #999, #818 ) ;
#407 = ORIENTED_EDGE ( 'NONE', *, *, #2177, .F. ) ;
#408 = DIRECTION ( 'NONE',  ( 0.000000000000000000, 0.000000000000000000, -1.000000000000000000 ) ) ;
#409 = DIRECTION ( 'NONE',  ( -0.000000000000000000, -1.000000000000000000, -0.000000000000000000 ) ) ;
#410 = CARTESIAN_POINT ( 'NONE',  ( 2.500000000000000000, -1.178949249685214307, 2.042000000000001592 ) ) ;
#411 = EDGE_LOOP ( 'NONE', ( #157, #890, #1925, #1517, #285 ) ) ;
#412 = CARTESIAN_POINT ( 'NONE',  ( -160.0000000000000284, 0.000000000000000000, 60.00000000000001421 ) ) ;
#413 = DIRECTION ( 'NONE',  ( -1.000000000000000000, -0.000000000000000000, -0.000000000000000000 ) ) ;
#414 = LINE ( 'NONE', #1587, #1253 ) ;
#415 = VERTEX_POINT ( 'NONE', #1060 ) ;
#416 = EDGE_CURVE ( 'NONE', #94, #899, #2141, .T. ) ;
#417 = EDGE_LOOP ( 'NONE', ( #282, #2155, #528, #1458 ) ) ;
#418 = VECTOR ( 'NONE', #409, 1000.000000000000000 ) ;
#419 = DIRECTION ( 'NONE',  ( 0.000000000000000000, 0.000000000000000000, 1.000000000000000000 ) ) ;
#420 = DIRECTION ( 'NONE',  ( 0.000000000000000000, -1.000000000000000000, 0.000000000000000000 ) ) ;
#421 = DIRECTION ( 'NONE',  ( -1.000000000000000000, 0.000000000000000000, 0.000000000000000000 ) ) ;
#422 = LINE ( 'NONE', #1104, #878 ) ;
#423 = ADVANCED_FACE ( 'NONE', ( #1755 ), #626, .F. ) ;
#424 = EDGE_CURVE ( 'NONE', #2192, #4, #546, .T. ) ;
#425 = PRODUCT_DEFINITION_SHAPE ( 'NONE', 'NONE',  #1410 ) ;
#426 = FACE_BOUND ( 'NONE', #2181, .T. ) ;
#427 = DIRECTION ( 'NONE',  ( 0.000000000000000000, -1.000000000000000000, 0.000000000000000000 ) ) ;
#428 =( LENGTH_UNIT ( ) NAMED_UNIT ( * ) SI_UNIT ( .MILLI., .METRE. ) );
#429 = VECTOR ( 'NONE', #1167, 1000.000000000000000 ) ;
#430 = ORIENTED_EDGE ( 'NONE', *, *, #1751, .F. ) ;
#431 = APPLICATION_CONTEXT ( 'automotive_design' ) ;
#432 = ORIENTED_EDGE ( 'NONE', *, *, #775, .T. ) ;
#433 = DIRECTION ( 'NONE',  ( 1.000000000000000000, 0.000000000000000000, 0.000000000000000000 ) ) ;
#434 = DIRECTION ( 'NONE',  ( 0.000000000000000000, 0.000000000000000000, -1.000000000000000000 ) ) ;
#436 = ORIENTED_EDGE ( 'NONE', *, *, #2067, .F. ) ;
#435 = DIRECTION ( 'NONE',  ( -0.5000000000000051070, 0.000000000000000000, 0.8660254037844355990 ) ) ;
#437 = AXIS2_PLACEMENT_3D ( 'NONE', #747, #702, #1251 ) ;
#438 = DIRECTION ( 'NONE',  ( 0.000000000000000000, -1.000000000000000000, 0.000000000000000000 ) ) ;
#439 = CARTESIAN_POINT ( 'NONE',  ( 2.500000000000000000, 0.000000000000000000, 0.000000000000000000 ) ) ;
#440 = EDGE_LOOP ( 'NONE', ( #687, #1990, #789, #2117 ) ) ;
#441 = AXIS2_PLACEMENT_3D ( 'NONE', #484, #315, #1178 ) ;
#442 = ORIENTED_EDGE ( 'NONE', *, *, #775, .F. ) ;
#443 = CARTESIAN_POINT ( 'NONE',  ( 145.0000000000000284, 2.993649167310367343, -42.35000000000001563 ) ) ;
#444 = CIRCLE ( 'NONE', #2022, 0.2000000000000000944 ) ;
#445 = ORIENTED_EDGE ( 'NONE', *, *, #1312, .T. ) ;
#447 = EDGE_LOOP ( 'NONE', ( #2179, #296 ) ) ;
#446 = DIRECTION ( 'NONE',  ( -1.000000000000000000, -0.000000000000000000, -0.000000000000000000 ) ) ;
#448 = CARTESIAN_POINT ( 'NONE',  ( -145.0000000000000284, 3.000000000000000000, 45.00000000000000000 ) ) ;
#449 = DIRECTION ( 'NONE',  ( 0.000000000000000000, 0.000000000000000000, -1.000000000000000000 ) ) ;
#450 = PLANE ( 'NONE',  #98 ) ;
#451 = ADVANCED_FACE ( 'NONE', ( #393 ), #1399, .F. ) ;
#452 = ORIENTED_EDGE ( 'NONE', *, *, #101, .T. ) ;
#453 = PRODUCT_DEFINITION ( 'UNKNOWN', '', #940, #1003 ) ;
#454 = ORIENTED_EDGE ( 'NONE', *, *, #1956, .T. ) ;
#455 = DIRECTION ( 'NONE',  ( 1.000000000000000000, 6.123233995736766036E-17, -1.224646799147353207E-16 ) ) ;
#456 = ORIENTED_EDGE ( 'NONE', *, *, #633, .T. ) ;
#457 = LINE ( 'NONE', #1731, #1139 ) ;
#458 = CARTESIAN_POINT ( 'NONE',  ( 145.0000000000000284, 2.993649167310367343, -45.00000000000000000 ) ) ;
#459 = DIRECTION ( 'NONE',  ( -0.000000000000000000, 1.000000000000000000, -0.000000000000000000 ) ) ;
#460 =( NAMED_UNIT ( * ) SI_UNIT ( $, .STERADIAN. ) SOLID_ANGLE_UNIT ( ) );
#461 = VECTOR ( 'NONE', #1047, 1000.000000000000000 ) ;
#462 = PRODUCT_DEFINITION_SHAPE ( 'NONE', 'NONE',  #2231 ) ;
#463 = VERTEX_POINT ( 'NONE', #1616 ) ;
#464 = CARTESIAN_POINT ( 'NONE',  ( 2.500000000000000000, 0.000000000000000000, 0.000000000000000000 ) ) ;
#465 = ORIENTED_EDGE ( 'NONE', *, *, #819, .F. ) ;
#466 = DIRECTION ( 'NONE',  ( -5.204170427930417339E-16, -1.000000000000000000, 0.000000000000000000 ) ) ;
#467 = EDGE_CURVE ( 'NONE', #486, #1704, #896, .T. ) ;
#468 = DIRECTION ( 'NONE',  ( 0.000000000000000000, 0.000000000000000000, -1.000000000000000000 ) ) ;
#469 = ADVANCED_FACE ( 'NONE', ( #782 ), #2081, .T. ) ;
#470 = CARTESIAN_POINT ( 'NONE',  ( 5.000000000000002665, 3.306546357697854226E-16, 2.700000000000000622 ) ) ;
#471 = CONTEXT_DEPENDENT_SHAPE_REPRESENTATION ( #5, #641 ) ;
#472 =( NAMED_UNIT ( * ) SI_UNIT ( $, .STERADIAN. ) SOLID_ANGLE_UNIT ( ) );
#473 = VERTEX_POINT ( 'NONE', #1228 ) ;
#474 = CARTESIAN_POINT ( 'NONE',  ( -145.0000000000000284, -3.358697307418414604E-14, -47.50000000000000000 ) ) ;
#475 = ORIENTED_EDGE ( 'NONE', *, *, #2178, .F. ) ;
#476 =( GEOMETRIC_REPRESENTATION_CONTEXT ( 3 ) GLOBAL_UNCERTAINTY_ASSIGNED_CONTEXT ( ( #681 ) ) GLOBAL_UNIT_ASSIGNED_CONTEXT ( ( #1535, #1035, #652 ) ) REPRESENTATION_CONTEXT ( 'NONE', 'WORKASPACE' ) );
#477 = EDGE_CURVE ( 'NONE', #333, #2156, #1577, .T. ) ;
#478 = CIRCLE ( 'NONE', #1724, 0.2500000000000002220 ) ;
#479 = DIRECTION ( 'NONE',  ( -0.000000000000000000, 1.000000000000000000, -0.000000000000000000 ) ) ;
#480 = VECTOR ( 'NONE', #596, 1000.000000000000000 ) ;
#481 = CARTESIAN_POINT ( 'NONE',  ( 0.2500000000000002220, 0.000000000000000000, 0.000000000000000000 ) ) ;
#482 = EDGE_CURVE ( 'NONE', #486, #1700, #1469, .T. ) ;
#483 = ORIENTED_EDGE ( 'NONE', *, *, #1734, .F. ) ;
#484 = CARTESIAN_POINT ( 'NONE',  ( 145.0000000000000284, 3.000000000000002665, 45.00000000000000000 ) ) ;
#485 = PLANE ( 'NONE',  #1391 ) ;
#486 = VERTEX_POINT ( 'NONE', #1921 ) ;
#487 = CARTESIAN_POINT ( 'NONE',  ( -160.0000000000000284, 10.00000000000000000, 60.00000000000001421 ) ) ;
#488 = ORIENTED_EDGE ( 'NONE', *, *, #2122, .T. ) ;
#489 = CARTESIAN_POINT ( 'NONE',  ( 0.000000000000000000, 1.178949249685212974, -2.042000000000001148 ) ) ;
#490 = CARTESIAN_POINT ( 'NONE',  ( 2.500000000000000000, 0.000000000000000000, 0.000000000000000000 ) ) ;
#491 = ORIENTED_EDGE ( 'NONE', *, *, #1236, .F. ) ;
#492 = CARTESIAN_POINT ( 'NONE',  ( -145.0000000000000284, -3.358697307418414604E-14, 42.49999999999999289 ) ) ;
#493 = CONICAL_SURFACE ( 'NONE', #1919, 2.055000000000000160, 0.7853981633974639331 ) ;
#494 = CARTESIAN_POINT ( 'NONE',  ( -160.0000000000000284, 10.00000000000000000, 60.00000000000001421 ) ) ;
#495 = DIRECTION ( 'NONE',  ( 0.000000000000000000, 0.000000000000000000, 1.000000000000000000 ) ) ;
#496 = AXIS2_PLACEMENT_3D ( 'NONE', #1411, #795, #99 ) ;
#497 = EDGE_LOOP ( 'NONE', ( #1053, #1791, #14, #2049 ) ) ;
#498 = ORIENTED_EDGE ( 'NONE', *, *, #929, .F. ) ;
#499 = DIRECTION ( 'NONE',  ( -1.000000000000000000, -0.000000000000000000, -0.000000000000000000 ) ) ;
#500 = DIRECTION ( 'NONE',  ( 0.000000000000000000, 0.000000000000000000, 1.000000000000000000 ) ) ;
#501 = VECTOR ( 'NONE', #330, 1000.000000000000000 ) ;
#502 = UNCERTAINTY_MEASURE_WITH_UNIT (LENGTH_MEASURE( 1.000000000000000082E-05 ), #1094, 'distance_accuracy_value', 'NONE');
#503 = ORIENTED_EDGE ( 'NONE', *, *, #1309, .T. ) ;
#504 = CARTESIAN_POINT ( 'NONE',  ( 0.2500000000000002220, 0.000000000000000000, 4.000000000000000000 ) ) ;
#505 = CARTESIAN_POINT ( 'NONE',  ( 5.200000000000002842, 0.000000000000000000, 0.000000000000000000 ) ) ;
#506 = VECTOR ( 'NONE', #299, 1000.000000000000114 ) ;
#507 = CIRCLE ( 'NONE', #242, 0.2000000000000000944 ) ;
#508 = CARTESIAN_POINT ( 'NONE',  ( -145.0000000000000284, 8.000000000000003553, 45.00000000000000000 ) ) ;
#509 = EDGE_CURVE ( 'NONE', #216, #1444, #1194, .T. ) ;
#510 = EDGE_LOOP ( 'NONE', ( #1989, #1715, #2217, #1147 ) ) ;
#511 = ORIENTED_EDGE ( 'NONE', *, *, #1169, .F. ) ;
#512 = FACE_OUTER_BOUND ( 'NONE', #1696, .T. ) ;
#513 = CARTESIAN_POINT ( 'NONE',  ( -145.0000000000000284, 2.800000000000000266, -47.70000000000000284 ) ) ;
#514 = MECHANICAL_DESIGN_GEOMETRIC_PRESENTATION_REPRESENTATION (  '', ( #1549 ), #297 ) ;
#515 = ORIENTED_EDGE ( 'NONE', *, *, #1804, .T. ) ;
#516 = DIRECTION ( 'NONE',  ( -0.000000000000000000, 1.000000000000000000, -0.000000000000000000 ) ) ;
#517 = VECTOR ( 'NONE', #953, 1000.000000000000000 ) ;
#518 = EDGE_CURVE ( 'NONE', #1097, #1470, #611, .T. ) ;
#519 = DIRECTION ( 'NONE',  ( 1.000000000000000000, 0.000000000000000000, 0.000000000000000000 ) ) ;
#520 = EDGE_CURVE ( 'NONE', #665, #473, #1798, .T. ) ;
#521 = ORIENTED_EDGE ( 'NONE', *, *, #477, .F. ) ;
#522 = EDGE_CURVE ( 'NONE', #1661, #415, #1521, .T. ) ;
#523 = ORIENTED_EDGE ( 'NONE', *, *, #197, .T. ) ;
#524 = DIRECTION ( 'NONE',  ( 0.000000000000000000, 0.000000000000000000, -1.000000000000000000 ) ) ;
#525 = DIRECTION ( 'NONE',  ( -1.000000000000000000, -0.000000000000000000, -0.000000000000000000 ) ) ;
#526 = DIRECTION ( 'NONE',  ( -1.000000000000000000, -0.000000000000000000, -0.000000000000000000 ) ) ;
#527 = VECTOR ( 'NONE', #1737, 1000.000000000000000 ) ;
#528 = ORIENTED_EDGE ( 'NONE', *, *, #186, .T. ) ;
#529 = CARTESIAN_POINT ( 'NONE',  ( -145.0000000000000284, 0.000000000000000000, 45.00000000000000000 ) ) ;
#530 = DIRECTION ( 'NONE',  ( 1.000000000000000000, 0.000000000000000000, 0.000000000000000000 ) ) ;
#531 = ADVANCED_FACE ( 'NONE', ( #1140 ), #1335, .F. ) ;
#532 = LINE ( 'NONE', #1215, #838 ) ;
#533 = AXIS2_PLACEMENT_3D ( 'NONE', #1446, #89, #1957 ) ;
#534 = ADVANCED_FACE ( 'NONE', ( #329 ), #855, .T. ) ;
#535 = CARTESIAN_POINT ( 'NONE',  ( 2.500000000000000000, -1.178949249685214307, 2.042000000000001592 ) ) ;
#536 = AXIS2_PLACEMENT_3D ( 'NONE', #928, #2126, #403 ) ;
#537 = VERTEX_POINT ( 'NONE', #292 ) ;
#538 = CARTESIAN_POINT ( 'NONE',  ( 2.500000000000000000, 0.000000000000000000, 0.000000000000000000 ) ) ;
#539 = DIRECTION ( 'NONE',  ( -2.312964634635742957E-16, 0.000000000000000000, 1.000000000000000000 ) ) ;
#540 = CARTESIAN_POINT ( 'NONE',  ( -149.9999999999999716, -120.0000000000000142, -50.00000000000000000 ) ) ;
#541 = EDGE_CURVE ( 'NONE', #899, #2107, #1532, .T. ) ;
#542 = DIRECTION ( 'NONE',  ( 0.000000000000000000, -1.000000000000000000, 0.000000000000000000 ) ) ;
#543 = EDGE_CURVE ( 'NONE', #1735, #1188, #1860, .T. ) ;
#544 =( GEOMETRIC_REPRESENTATION_CONTEXT ( 3 ) GLOBAL_UNCERTAINTY_ASSIGNED_CONTEXT ( ( #161 ) ) GLOBAL_UNIT_ASSIGNED_CONTEXT ( ( #96, #1865, #2034 ) ) REPRESENTATION_CONTEXT ( 'NONE', 'WORKASPACE' ) );
#545 = VECTOR ( 'NONE', #1920, 1000.000000000000000 ) ;
#546 = LINE ( 'NONE', #1743, #1551 ) ;
#547 = CARTESIAN_POINT ( 'NONE',  ( 2.500000000000000000, -1.178949249685214307, 2.042000000000001592 ) ) ;
#548 = VECTOR ( 'NONE', #1691, 1000.000000000000000 ) ;
#549 = ORIENTED_EDGE ( 'NONE', *, *, #616, .T. ) ;
#550 = ORIENTED_EDGE ( 'NONE', *, *, #1571, .T. ) ;
#551 = DIRECTION ( 'NONE',  ( 0.000000000000000000, -1.000000000000000000, 1.287488025362403787E-15 ) ) ;
#552 = CARTESIAN_POINT ( 'NONE',  ( -145.0000000000000284, 2.993649167310367343, -45.00000000000000000 ) ) ;
#553 = PLANE ( 'NONE',  #1005 ) ;
#554 = CARTESIAN_POINT ( 'NONE',  ( -31.74999999999995737, 0.000000000000000000, 4.250000000000000000 ) ) ;
#555 = CARTESIAN_POINT ( 'NONE',  ( 4.999999999999997335, 0.000000000000000000, 4.250000000000000000 ) ) ;
#556 = CARTESIAN_POINT ( 'NONE',  ( 2.500000000000000000, 1.178949249685217415, 2.041999999999998483 ) ) ;
#557 = VECTOR ( 'NONE', #16, 1000.000000000000000 ) ;
#558 = ORIENTED_EDGE ( 'NONE', *, *, #378, .F. ) ;
#559 = EDGE_CURVE ( 'NONE', #610, #1963, #1824, .T. ) ;
#560 = ORIENTED_EDGE ( 'NONE', *, *, #686, .T. ) ;
#561 = CARTESIAN_POINT ( 'NONE',  ( -139.9999999999999716, -120.0000000000000142, 50.00000000000000000 ) ) ;
#562 = CARTESIAN_POINT ( 'NONE',  ( 21.00000000000000355, 2.789133085058097101E-16, -2.055000000000000160 ) ) ;
#563 = LINE ( 'NONE', #410, #1905 ) ;
#564 = TOROIDAL_SURFACE ( 'NONE', #51, 2.700000000000000622, 0.2000000000000000111 ) ;
#565 = PLANE ( 'NONE',  #302 ) ;
#566 = LINE ( 'NONE', #1777, #1649 ) ;
#567 = EDGE_CURVE ( 'NONE', #1735, #240, #1938, .T. ) ;
#568 = ORIENTED_EDGE ( 'NONE', *, *, #1707, .T. ) ;
#569 = AXIS2_PLACEMENT_3D ( 'NONE', #1832, #466, #839 ) ;
#570 = AXIS2_PLACEMENT_3D ( 'NONE', #912, #1927, #1770 ) ;
#571 = EDGE_LOOP ( 'NONE', ( #498, #1915, #1230, #1366 ) ) ;
#572 = CARTESIAN_POINT ( 'NONE',  ( -145.0000000000000284, 0.000000000000000000, -42.35000000000001563 ) ) ;
#573 = CARTESIAN_POINT ( 'NONE',  ( -150.0000000000000284, -9.999999999999994671, -40.00000000000000000 ) ) ;
#574 = CARTESIAN_POINT ( 'NONE',  ( -145.0000000000000284, 2.993649167310367343, 42.35000000000001563 ) ) ;
#575 = VERTEX_POINT ( 'NONE', #2029 ) ;
#576 = LINE ( 'NONE', #1260, #2086 ) ;
#577 = LINE ( 'NONE', #231, #1370 ) ;
#578 = PLANE ( 'NONE',  #1787 ) ;
#579 = AXIS2_PLACEMENT_3D ( 'NONE', #9, #516, #20 ) ;
#580 = EDGE_CURVE ( 'NONE', #898, #1725, #31, .T. ) ;
#581 = VECTOR ( 'NONE', #59, 1000.000000000000000 ) ;
#582 = CARTESIAN_POINT ( 'NONE',  ( -145.0000000000000284, 2.993649167310367343, -45.00000000000000000 ) ) ;
#583 = AXIS2_PLACEMENT_3D ( 'NONE', #756, #260, #1459 ) ;
#584 = ORIENTED_EDGE ( 'NONE', *, *, #55, .T. ) ;
#585 = CARTESIAN_POINT ( 'NONE',  ( 2.500000000000000000, 1.178949249685212974, -2.042000000000001148 ) ) ;
#586 = EDGE_CURVE ( 'NONE', #1579, #80, #478, .T. ) ;
#587 = DIRECTION ( 'NONE',  ( 0.000000000000000000, 0.8660254037844380415, -0.5000000000000012212 ) ) ;
#588 = FACE_OUTER_BOUND ( 'NONE', #607, .T. ) ;
#589 =( NAMED_UNIT ( * ) PLANE_ANGLE_UNIT ( ) SI_UNIT ( $, .RADIAN. ) );
#590 = FACE_BOUND ( 'NONE', #2014, .T. ) ;
#591 = DIRECTION ( 'NONE',  ( 0.000000000000000000, 0.000000000000000000, 1.000000000000000000 ) ) ;
#592 = ORIENTED_EDGE ( 'NONE', *, *, #482, .T. ) ;
#593 = ORIENTED_EDGE ( 'NONE', *, *, #2015, .T. ) ;
#594 = AXIS2_PLACEMENT_3D ( 'NONE', #1603, #1291, #433 ) ;
#595 = CYLINDRICAL_SURFACE ( 'NONE', #1464, 2.649999999999985700 ) ;
#596 = DIRECTION ( 'NONE',  ( 0.000000000000000000, 1.000000000000000000, -1.287488025362403787E-15 ) ) ;
#598 = ORIENTED_EDGE ( 'NONE', *, *, #111, .F. ) ;
#597 = LINE ( 'NONE', #1968, #1856 ) ;
#599 = SURFACE_SIDE_STYLE ('',( #1595 ) ) ;
#600 = CIRCLE ( 'NONE', #277, 2.041999999999999815 ) ;
#601 = PRODUCT_DEFINITION_SHAPE ( 'NONE', 'NONE',  #2232 ) ;
#602 = CARTESIAN_POINT ( 'NONE',  ( 5.200000000000002842, 3.061616997868383634E-16, -2.500000000000000444 ) ) ;
#603 = DIRECTION ( 'NONE',  ( 1.000000000000000000, 0.000000000000000000, 0.000000000000000000 ) ) ;
#604 = EDGE_CURVE ( 'NONE', #776, #1816, #1996, .T. ) ;
#605 = AXIS2_PLACEMENT_3D ( 'NONE', #505, #17, #2030 ) ;
#606 = ORIENTED_EDGE ( 'NONE', *, *, #850, .F. ) ;
#607 = EDGE_LOOP ( 'NONE', ( #2150, #1303, #1866, #1115 ) ) ;
#608 = CARTESIAN_POINT ( 'NONE',  ( 5.200000000000002842, 0.000000000000000000, -2.700000000000000622 ) ) ;
#609 = CARTESIAN_POINT ( 'NONE',  ( 4.999999999999997335, 0.000000000000000000, 0.000000000000000000 ) ) ;
#610 = VERTEX_POINT ( 'NONE', #119 ) ;
#612 = ORIENTED_EDGE ( 'NONE', *, *, #1333, .F. ) ;
#611 = LINE ( 'NONE', #1980, #370 ) ;
#613 = DIRECTION ( 'NONE',  ( 0.000000000000000000, 0.000000000000000000, -1.000000000000000000 ) ) ;
#614 = CARTESIAN_POINT ( 'NONE',  ( 5.000000000000000888, 4.250000000000000000, 0.000000000000000000 ) ) ;
#615 = FACE_BOUND ( 'NONE', #447, .T. ) ;
#616 = EDGE_CURVE ( 'NONE', #65, #145, #672, .T. ) ;
#617 = APPLICATION_PROTOCOL_DEFINITION ( 'draft international standard', 'automotive_design', 1998, #431 ) ;
#618 =( LENGTH_UNIT ( ) NAMED_UNIT ( * ) SI_UNIT ( .MILLI., .METRE. ) );
#619 = ORIENTED_EDGE ( 'NONE', *, *, #914, .T. ) ;
#620 = COLOUR_RGB ( '',1.000000000000000000, 0.9490196078431372140, 0.9098039215686274384 ) ;
#621 = VECTOR ( 'NONE', #683, 1000.000000000000000 ) ;
#622 = EDGE_LOOP ( 'NONE', ( #2158, #682, #110, #1343, #549 ) ) ;
#623 = FACE_OUTER_BOUND ( 'NONE', #1302, .T. ) ;
#624 = AXIS2_PLACEMENT_3D ( 'NONE', #481, #138, #2017 ) ;
#625 = VERTEX_POINT ( 'NONE', #492 ) ;
#627 = VERTEX_POINT ( 'NONE', #470 ) ;
#626 = PLANE ( 'NONE',  #785 ) ;
#628 = LINE ( 'NONE', #1308, #2032 ) ;
#629 = DIRECTION ( 'NONE',  ( -1.000000000000000000, -0.000000000000000000, -0.000000000000000000 ) ) ;
#630 = ITEM_DEFINED_TRANSFORMATION ( 'NONE', 'NONE', #1262,  #30 ) ;
#631 = ORIENTED_EDGE ( 'NONE', *, *, #1970, .T. ) ;
#632 = CARTESIAN_POINT ( 'NONE',  ( 145.0000000000000284, 2.800000000000000266, -42.29999999999999716 ) ) ;
#633 = EDGE_CURVE ( 'NONE', #860, #2107, #1339, .T. ) ;
#634 = ORIENTED_EDGE ( 'NONE', *, *, #1668, .T. ) ;
#635 = CIRCLE ( 'NONE', #1354, 2.700000000000001066 ) ;
#636 = LINE ( 'NONE', #1138, #1369 ) ;
#637 = FACE_OUTER_BOUND ( 'NONE', #933, .T. ) ;
#638 = CARTESIAN_POINT ( 'NONE',  ( -145.0000000000000284, 3.000000000000000000, 42.35000000000001563 ) ) ;
#639 = DIRECTION ( 'NONE',  ( -2.312964634635740985E-16, 1.000000000000000000, 0.000000000000000000 ) ) ;
#640 = AXIS2_PLACEMENT_3D ( 'NONE', #2075, #1219, #346 ) ;
#641 = PRODUCT_DEFINITION_SHAPE ( 'NONE', 'NONE',  #2228 ) ;
#642 = PRESENTATION_STYLE_ASSIGNMENT (( #264 ) ) ;
#643 = VERTEX_POINT ( 'NONE', #2041 ) ;
#644 = CONICAL_SURFACE ( 'NONE', #536, 2.500000000000002220, 1.029744258676654534 ) ;
#645 = EDGE_CURVE ( 'NONE', #1390, #267, #657, .T. ) ;
#646 = CARTESIAN_POINT ( 'NONE',  ( 0.000000000000000000, 0.000000000000000000, 40.00000000000000000 ) ) ;
#647 = EDGE_LOOP ( 'NONE', ( #1594, #634, #74, #1929 ) ) ;
#648 = CARTESIAN_POINT ( 'NONE',  ( 2.500000000000000000, 1.178949249685212974, -2.042000000000001148 ) ) ;
#649 = DIRECTION ( 'NONE',  ( 0.000000000000000000, 0.000000000000000000, 1.000000000000000000 ) ) ;
#650 = CARTESIAN_POINT ( 'NONE',  ( 145.0000000000000284, 3.000000000000000000, 42.35000000000001563 ) ) ;
#651 = DIRECTION ( 'NONE',  ( 0.000000000000000000, -0.000000000000000000, -1.000000000000000000 ) ) ;
#652 =( NAMED_UNIT ( * ) SI_UNIT ( $, .STERADIAN. ) SOLID_ANGLE_UNIT ( ) );
#653 = VERTEX_POINT ( 'NONE', #2223 ) ;
#654 = FACE_OUTER_BOUND ( 'NONE', #571, .T. ) ;
#655 = ORIENTED_EDGE ( 'NONE', *, *, #2083, .F. ) ;
#656 = PRODUCT_DEFINITION_FORMATION_WITH_SPECIFIED_SOURCE ( 'ANY', '', #1962, .NOT_KNOWN. ) ;
#657 = CIRCLE ( 'NONE', #298, 2.700000000000001066 ) ;
#658 = DIRECTION ( 'NONE',  ( 6.123233995736766036E-17, -1.000000000000000000, 0.000000000000000000 ) ) ;
#659 = CIRCLE ( 'NONE', #2087, 2.700000000000001066 ) ;
#660 = DIRECTION ( 'NONE',  ( -1.000000000000000000, -0.000000000000000000, -0.000000000000000000 ) ) ;
#661 = ORIENTED_EDGE ( 'NONE', *, *, #424, .T. ) ;
#662 = DIRECTION ( 'NONE',  ( -1.000000000000000000, -0.000000000000000000, -0.000000000000000000 ) ) ;
#663 = DIRECTION ( 'NONE',  ( -2.312964634635742957E-16, 1.000000000000000000, 0.000000000000000000 ) ) ;
#664 =( NAMED_UNIT ( * ) PLANE_ANGLE_UNIT ( ) SI_UNIT ( $, .RADIAN. ) );
#665 = VERTEX_POINT ( 'NONE', #1701 ) ;
#666 = LINE ( 'NONE', #1830, #1584 ) ;
#667 = ORIENTED_EDGE ( 'NONE', *, *, #1241, .T. ) ;
#668 = DIRECTION ( 'NONE',  ( -6.123233995736766036E-17, 1.000000000000000000, -0.000000000000000000 ) ) ;
#669 = DIRECTION ( 'NONE',  ( 4.336808689942017736E-17, -0.000000000000000000, 1.000000000000000000 ) ) ;
#670 = EDGE_CURVE ( 'NONE', #575, #1569, #809, .T. ) ;
#671 = VERTEX_POINT ( 'NONE', #991 ) ;
#672 = LINE ( 'NONE', #303, #1619 ) ;
#673 = CONICAL_SURFACE ( 'NONE', #1774, 2.041999999999999815, 1.047197551196591858 ) ;
#674 = DIRECTION ( 'NONE',  ( 0.000000000000000000, 0.000000000000000000, 1.000000000000000000 ) ) ;
#675 = VECTOR ( 'NONE', #752, 1000.000000000000000 ) ;
#676 = EDGE_LOOP ( 'NONE', ( #430, #86, #1552, #1065 ) ) ;
#677 = ORIENTED_EDGE ( 'NONE', *, *, #879, .F. ) ;
#678 = DIRECTION ( 'NONE',  ( 0.000000000000000000, 0.000000000000000000, 1.000000000000000000 ) ) ;
#679 = DIRECTION ( 'NONE',  ( -0.000000000000000000, 0.8660254037844392627, 0.4999999999999990008 ) ) ;
#680 = VECTOR ( 'NONE', #244, 1000.000000000000000 ) ;
#681 = UNCERTAINTY_MEASURE_WITH_UNIT (LENGTH_MEASURE( 1.000000000000000082E-05 ), #1535, 'distance_accuracy_value', 'NONE');
#682 = ORIENTED_EDGE ( 'NONE', *, *, #13, .F. ) ;
#683 = DIRECTION ( 'NONE',  ( -1.000000000000000000, -0.000000000000000000, 4.336808689942017736E-17 ) ) ;
#684 = EDGE_CURVE ( 'NONE', #267, #1390, #942, .T. ) ;
#685 = AXIS2_PLACEMENT_3D ( 'NONE', #778, #2119, #209 ) ;
#686 = EDGE_CURVE ( 'NONE', #1439, #835, #831, .T. ) ;
#687 = ORIENTED_EDGE ( 'NONE', *, *, #1542, .F. ) ;
#688 = ORIENTED_EDGE ( 'NONE', *, *, #1935, .F. ) ;
#689 = CARTESIAN_POINT ( 'NONE',  ( -145.0000000000000284, 3.000000000000000000, 47.64999999999998437 ) ) ;
#690 = FACE_OUTER_BOUND ( 'NONE', #1015, .T. ) ;
#691 = AXIS2_PLACEMENT_3D ( 'NONE', #1851, #1351, #519 ) ;
#692 = DIRECTION ( 'NONE',  ( 1.000000000000000000, 0.000000000000000000, 0.000000000000000000 ) ) ;
#693 = CIRCLE ( 'NONE', #583, 0.2000000000000000944 ) ;
#694 = VERTEX_POINT ( 'NONE', #339 ) ;
#695 = ORIENTED_EDGE ( 'NONE', *, *, #850, .T. ) ;
#696 = EDGE_CURVE ( 'NONE', #324, #1887, #700, .T. ) ;
#697 = DIRECTION ( 'NONE',  ( 0.000000000000000000, -1.000000000000000000, 0.000000000000000000 ) ) ;
#698 = EDGE_CURVE ( 'NONE', #705, #1125, #1513, .T. ) ;
#699 = DIRECTION ( 'NONE',  ( 0.000000000000000000, -0.8660254037844390407, -0.4999999999999993339 ) ) ;
#700 = LINE ( 'NONE', #1557, #545 ) ;
#701 = CIRCLE ( 'NONE', #816, 2.649999999999985700 ) ;
#702 = DIRECTION ( 'NONE',  ( 1.000000000000000000, -0.000000000000000000, 2.312964634635742957E-16 ) ) ;
#703 = EDGE_CURVE ( 'NONE', #333, #643, #1576, .T. ) ;
#704 = TOROIDAL_SURFACE ( 'NONE', #859, 2.700000000000000622, 0.2000000000000000111 ) ;
#705 = VERTEX_POINT ( 'NONE', #191 ) ;
#706 = EDGE_CURVE ( 'NONE', #1353, #1358, #1157, .T. ) ;
#707 = CARTESIAN_POINT ( 'NONE',  ( 145.0000000000000284, 3.000000000000001776, 42.29999999999999716 ) ) ;
#708 = FACE_OUTER_BOUND ( 'NONE', #1170, .T. ) ;
#709 = CARTESIAN_POINT ( 'NONE',  ( -139.9999999999999716, -120.0000000000000142, 50.00000000000000000 ) ) ;
#710 = ORIENTED_EDGE ( 'NONE', *, *, #1596, .F. ) ;
#711 = CARTESIAN_POINT ( 'NONE',  ( 0.000000000000000000, -1.178949249685214307, 2.042000000000001592 ) ) ;
#712 = VECTOR ( 'NONE', #893, 1000.000000000000000 ) ;
#713 = CARTESIAN_POINT ( 'NONE',  ( -31.74999999999995737, 0.000000000000000000, 0.000000000000000000 ) ) ;
#714 = AXIS2_PLACEMENT_3D ( 'NONE', #1093, #262, #1427 ) ;
#715 = EDGE_LOOP ( 'NONE', ( #1004, #870, #1543 ) ) ;
#716 = ORIENTED_EDGE ( 'NONE', *, *, #580, .F. ) ;
#717 = DIRECTION ( 'NONE',  ( 6.123233995736766036E-17, -1.000000000000000000, 0.000000000000000000 ) ) ;
#718 = CARTESIAN_POINT ( 'NONE',  ( -145.0000000000000284, 3.000000000000002665, -45.00000000000000000 ) ) ;
#719 = LINE ( 'NONE', #821, #2072 ) ;
#720 = DIRECTION ( 'NONE',  ( 0.000000000000000000, 0.000000000000000000, -1.000000000000000000 ) ) ;
#721 = COLOUR_RGB ( '',0.8941176470588234615, 0.8941176470588234615, 0.8941176470588234615 ) ;
#722 = VECTOR ( 'NONE', #1033, 1000.000000000000000 ) ;
#723 = DIRECTION ( 'NONE',  ( 0.000000000000000000, -1.000000000000000000, 0.000000000000000000 ) ) ;
#724 = MECHANICAL_DESIGN_GEOMETRIC_PRESENTATION_REPRESENTATION (  '', ( #341 ), #117 ) ;
#725 = SURFACE_STYLE_FILL_AREA ( #22 ) ;
#726 = TOROIDAL_SURFACE ( 'NONE', #2121, 2.700000000000000622, 0.2000000000000000111 ) ;
#727 = CARTESIAN_POINT ( 'NONE',  ( -145.0000000000000284, -15.00000000000003197, -47.50000000000000000 ) ) ;
#728 = ORIENTED_EDGE ( 'NONE', *, *, #10, .F. ) ;
#729 = ORIENTED_EDGE ( 'NONE', *, *, #1681, .F. ) ;
#730 = DIRECTION ( 'NONE',  ( -0.5000000000000051070, 1.060575238724903217E-16, -0.8660254037844355990 ) ) ;
#731 = DIRECTION ( 'NONE',  ( 0.000000000000000000, -1.000000000000000000, 0.000000000000000000 ) ) ;
#732 = FACE_OUTER_BOUND ( 'NONE', #375, .T. ) ;
#733 = CYLINDRICAL_SURFACE ( 'NONE', #1554, 2.649999999999985700 ) ;
#734 = EDGE_CURVE ( 'NONE', #610, #1465, #1834, .T. ) ;
#735 = PRESENTATION_STYLE_ASSIGNMENT (( #394 ) ) ;
#736 = ORIENTED_EDGE ( 'NONE', *, *, #266, .F. ) ;
#737 =( REPRESENTATION_RELATIONSHIP ('NONE','NONE', #367, #354 ) REPRESENTATION_RELATIONSHIP_WITH_TRANSFORMATION ( #1142 )SHAPE_REPRESENTATION_RELATIONSHIP( ) );
#738 = VERTEX_POINT ( 'NONE', #1409 ) ;
#739 = CARTESIAN_POINT ( 'NONE',  ( -145.0000000000000284, -3.353798720221824946E-14, -45.00000000000000000 ) ) ;
#740 = DIRECTION ( 'NONE',  ( -1.000000000000000000, -0.000000000000000000, -0.000000000000000000 ) ) ;
#741 = DIRECTION ( 'NONE',  ( -0.000000000000000000, 1.000000000000000000, -0.000000000000000000 ) ) ;
#742 = VECTOR ( 'NONE', #1443, 1000.000000000000000 ) ;
#743 = DIRECTION ( 'NONE',  ( -0.7071067811865364705, 0.000000000000000000, 0.7071067811865584529 ) ) ;
#744 = EDGE_CURVE ( 'NONE', #166, #1963, #2116, .T. ) ;
#745 = LINE ( 'NONE', #954, #2113 ) ;
#746 = EDGE_CURVE ( 'NONE', #220, #1505, #1729, .T. ) ;
#747 = CARTESIAN_POINT ( 'NONE',  ( -157.0000000000000284, 10.00000000000000000, 60.00000000000001421 ) ) ;
#748 = EDGE_CURVE ( 'NONE', #2144, #1284, #1372, .T. ) ;
#749 = VERTEX_POINT ( 'NONE', #1910 ) ;
#750 = CONICAL_SURFACE ( 'NONE', #977, 2.041999999999999815, 1.047197551196591858 ) ;
#751 = ORIENTED_EDGE ( 'NONE', *, *, #543, .F. ) ;
#752 = DIRECTION ( 'NONE',  ( -0.000000000000000000, 1.000000000000000000, -0.000000000000000000 ) ) ;
#753 = FACE_OUTER_BOUND ( 'NONE', #95, .T. ) ;
#754 = PLANE ( 'NONE',  #1436 ) ;
#755 = ORIENTED_EDGE ( 'NONE', *, *, #604, .F. ) ;
#756 = CARTESIAN_POINT ( 'NONE',  ( 145.0000000000000284, 2.800000000000000266, 42.29999999999999716 ) ) ;
#757 = FACE_OUTER_BOUND ( 'NONE', #162, .T. ) ;
#758 = CARTESIAN_POINT ( 'NONE',  ( -149.9999999999999716, -120.0000000000000142, -40.00000000000000000 ) ) ;
#759 = VECTOR ( 'NONE', #1013, 1000.000000000000000 ) ;
#760 = AXIS2_PLACEMENT_3D ( 'NONE', #1426, #219, #779 ) ;
#761 = ORIENTED_EDGE ( 'NONE', *, *, #1596, .T. ) ;
#762 = ORIENTED_EDGE ( 'NONE', *, *, #1790, .T. ) ;
#763 = DIRECTION ( 'NONE',  ( -0.000000000000000000, -0.000000000000000000, 1.000000000000000000 ) ) ;
#764 = DIRECTION ( 'NONE',  ( 0.000000000000000000, -0.5000000000000009992, -0.8660254037844380415 ) ) ;
#765 = EDGE_CURVE ( 'NONE', #405, #1579, #380, .T. ) ;
#766 = ORIENTED_EDGE ( 'NONE', *, *, #903, .F. ) ;
#767 = EDGE_CURVE ( 'NONE', #1725, #1444, #1884, .T. ) ;
#769 = ORIENTED_EDGE ( 'NONE', *, *, #283, .F. ) ;
#768 = DIRECTION ( 'NONE',  ( 1.000000000000000000, 0.000000000000000000, 0.000000000000000000 ) ) ;
#770 = DIRECTION ( 'NONE',  ( 2.312964634635742957E-16, 0.000000000000000000, -1.000000000000000000 ) ) ;
#771 = PLANE ( 'NONE',  #1011 ) ;
#772 = LINE ( 'NONE', #1447, #1746 ) ;
#773 = PRODUCT_CONTEXT ( 'NONE', #320, 'mechanical' ) ;
#774 = ORIENTED_EDGE ( 'NONE', *, *, #698, .T. ) ;
#775 = EDGE_CURVE ( 'NONE', #1348, #537, #1235, .T. ) ;
#776 = VERTEX_POINT ( 'NONE', #1069 ) ;
#777 = AXIS2_PLACEMENT_3D ( 'NONE', #102, #669, #114 ) ;
#778 = CARTESIAN_POINT ( 'NONE',  ( 2.500000000000000000, 2.357898499370431722, -2.818925648462311528E-15 ) ) ;
#779 = DIRECTION ( 'NONE',  ( 1.000000000000000000, 0.000000000000000000, -4.336808689942017736E-17 ) ) ;
#780 = ORIENTED_EDGE ( 'NONE', *, *, #1422, .T. ) ;
#781 = EDGE_CURVE ( 'NONE', #1255, #1661, #1741, .T. ) ;
#783 = EDGE_LOOP ( 'NONE', ( #1396, #1637, #1789, #387 ) ) ;
#782 = FACE_OUTER_BOUND ( 'NONE', #1808, .T. ) ;
#784 = DIRECTION ( 'NONE',  ( 0.000000000000000000, 0.000000000000000000, 1.000000000000000000 ) ) ;
#785 = AXIS2_PLACEMENT_3D ( 'NONE', #2159, #1114, #1630 ) ;
#786 = FACE_OUTER_BOUND ( 'NONE', #1740, .T. ) ;
#787 = DIRECTION ( 'NONE',  ( 0.000000000000000000, -1.000000000000000000, 0.000000000000000000 ) ) ;
#788 = VECTOR ( 'NONE', #1825, 1000.000000000000000 ) ;
#789 = ORIENTED_EDGE ( 'NONE', *, *, #1610, .T. ) ;
#790 = ORIENTED_EDGE ( 'NONE', *, *, #144, .F. ) ;
#791 = DIRECTION ( 'NONE',  ( -0.000000000000000000, -0.000000000000000000, -1.000000000000000000 ) ) ;
#792 = ORIENTED_EDGE ( 'NONE', *, *, #910, .F. ) ;
#793 = TOROIDAL_SURFACE ( 'NONE', #1252, 4.000000000000000000, 0.2500000000000000000 ) ;
#794 = VECTOR ( 'NONE', #237, 1000.000000000000000 ) ;
#796 = ORIENTED_EDGE ( 'NONE', *, *, #101, .F. ) ;
#795 = DIRECTION ( 'NONE',  ( -0.000000000000000000, 1.000000000000000000, -0.000000000000000000 ) ) ;
#797 = CARTESIAN_POINT ( 'NONE',  ( -145.0000000000000284, -3.353798720221824946E-14, -45.00000000000000000 ) ) ;
#798 = DIRECTION ( 'NONE',  ( -1.000000000000000000, -0.000000000000000000, -0.000000000000000000 ) ) ;
#799 = LINE ( 'NONE', #293, #23 ) ;
#800 = SHAPE_DEFINITION_REPRESENTATION ( #279, #261 ) ;
#801 = ADVANCED_FACE ( 'NONE', ( #368 ), #944, .F. ) ;
#802 = EDGE_LOOP ( 'NONE', ( #2028, #962, #952, #2198 ) ) ;
#803 = DIRECTION ( 'NONE',  ( 1.000000000000000000, 2.312964634635740985E-16, 0.000000000000000000 ) ) ;
#804 = TOROIDAL_SURFACE ( 'NONE', #2123, 2.700000000000000622, 0.2000000000000000111 ) ;
#805 = VERTEX_POINT ( 'NONE', #1753 ) ;
#806 = PRODUCT_DEFINITION_SHAPE ( 'NONE', 'NONE',  #822 ) ;
#807 = CARTESIAN_POINT ( 'NONE',  ( -145.0000000000000284, -3.353798720221824946E-14, 45.00000000000000000 ) ) ;
#808 = DIRECTION ( 'NONE',  ( 1.000000000000000000, 0.000000000000000000, 0.000000000000000000 ) ) ;
#809 = LINE ( 'NONE', #1871, #1902 ) ;
#810 = LINE ( 'NONE', #2127, #825 ) ;
#811 = ITEM_DEFINED_TRANSFORMATION ( 'NONE', 'NONE', #300,  #30 ) ;
#812 =( NAMED_UNIT ( * ) SI_UNIT ( $, .STERADIAN. ) SOLID_ANGLE_UNIT ( ) );
#813 = ORIENTED_EDGE ( 'NONE', *, *, #1708, .T. ) ;
#814 = LINE ( 'NONE', #974, #1051 ) ;
#815 = ORIENTED_EDGE ( 'NONE', *, *, #1007, .F. ) ;
#816 = AXIS2_PLACEMENT_3D ( 'NONE', #458, #980, #808 ) ;
#817 = CARTESIAN_POINT ( 'NONE',  ( -145.0000000000000284, 3.000000000000001776, 42.29999999999999716 ) ) ;
#818 = DIRECTION ( 'NONE',  ( 0.000000000000000000, 0.000000000000000000, 1.000000000000000000 ) ) ;
#819 = EDGE_CURVE ( 'NONE', #1531, #665, #1586, .T. ) ;
#820 = DIRECTION ( 'NONE',  ( 0.000000000000000000, 0.000000000000000000, -1.000000000000000000 ) ) ;
#821 = CARTESIAN_POINT ( 'NONE',  ( -140.0000000000000000, -10.00000000000000000, -40.00000000000000000 ) ) ;
#822 = PRODUCT_DEFINITION ( 'UNKNOWN', '', #1222, #1023 ) ;
#823 = EDGE_CURVE ( 'NONE', #94, #860, #41, .T. ) ;
#824 = ORIENTED_EDGE ( 'NONE', *, *, #2083, .T. ) ;
#825 = VECTOR ( 'NONE', #1987, 1000.000000000000114 ) ;
#826 = CYLINDRICAL_SURFACE ( 'NONE', #2161, 2.649999999999985700 ) ;
#827 = ORIENTED_EDGE ( 'NONE', *, *, #543, .T. ) ;
#828 = CARTESIAN_POINT ( 'NONE',  ( 0.000000000000000000, 0.000000000000000000, 4.000000000000000000 ) ) ;
#829 = FACE_OUTER_BOUND ( 'NONE', #1137, .T. ) ;
#830 = VERTEX_POINT ( 'NONE', #360 ) ;
#831 = LINE ( 'NONE', #1510, #621 ) ;
#832 = DIRECTION ( 'NONE',  ( 1.000000000000000000, 2.312964634635743450E-16, -0.000000000000000000 ) ) ;
#833 = VERTEX_POINT ( 'NONE', #1379 ) ;
#834 = CARTESIAN_POINT ( 'NONE',  ( -150.0000000000000000, 0.000000000000000000, 50.00000000000000000 ) ) ;
#835 = VERTEX_POINT ( 'NONE', #1545 ) ;
#836 = PRODUCT_DEFINITION_FORMATION_WITH_SPECIFIED_SOURCE ( 'ANY', '', #967, .NOT_KNOWN. ) ;
#837 = VECTOR ( 'NONE', #173, 1000.000000000000000 ) ;
#838 = VECTOR ( 'NONE', #1899, 1000.000000000000114 ) ;
#839 = DIRECTION ( 'NONE',  ( 1.000000000000000000, -5.204170427930417339E-16, 0.000000000000000000 ) ) ;
#840 = CIRCLE ( 'NONE', #1408, 4.250000000000000000 ) ;
#841 = DIRECTION ( 'NONE',  ( 1.000000000000000000, -5.204170427930417339E-16, 0.000000000000000000 ) ) ;
#842 = UNCERTAINTY_MEASURE_WITH_UNIT (LENGTH_MEASURE( 1.000000000000000082E-05 ), #1606, 'distance_accuracy_value', 'NONE');
#843 = EDGE_LOOP ( 'NONE', ( #1841, #386, #49, #1490 ) ) ;
#844 = CARTESIAN_POINT ( 'NONE',  ( 2.500000000000000000, 2.357898499370431722, -2.818925648462311528E-15 ) ) ;
#845 = DIRECTION ( 'NONE',  ( -0.000000000000000000, 1.000000000000000000, -0.000000000000000000 ) ) ;
#846 = CARTESIAN_POINT ( 'NONE',  ( -145.0000000000000284, 8.000000000000003553, -45.00000000000000000 ) ) ;
#847 = VERTEX_POINT ( 'NONE', #1207 ) ;
#848 = VERTEX_POINT ( 'NONE', #181 ) ;
#849 = APPLICATION_CONTEXT ( 'automotive_design' ) ;
#850 = EDGE_CURVE ( 'NONE', #473, #2218, #1945, .T. ) ;
#851 = DIRECTION ( 'NONE',  ( -1.000000000000000000, -0.000000000000000000, -0.000000000000000000 ) ) ;
#852 = DIRECTION ( 'NONE',  ( -1.000000000000000000, -0.000000000000000000, -0.000000000000000000 ) ) ;
#853 = PRODUCT_RELATED_PRODUCT_CATEGORY ( 'part', '', ( #1962 ) ) ;
#854 = ORIENTED_EDGE ( 'NONE', *, *, #1315, .T. ) ;
#855 = CYLINDRICAL_SURFACE ( 'NONE', #1050, 4.250000000000000000 ) ;
#856 = CIRCLE ( 'NONE', #2065, 0.2000000000000000944 ) ;
#857 = DIRECTION ( 'NONE',  ( 1.000000000000000000, 0.000000000000000000, 0.000000000000000000 ) ) ;
#858 = SURFACE_STYLE_FILL_AREA ( #1362 ) ;
#859 = AXIS2_PLACEMENT_3D ( 'NONE', #1196, #717, #365 ) ;
#860 = VERTEX_POINT ( 'NONE', #2070 ) ;
#861 = ORIENTED_EDGE ( 'NONE', *, *, #2166, .T. ) ;
#862 = DIRECTION ( 'NONE',  ( -0.000000000000000000, 1.000000000000000000, -0.000000000000000000 ) ) ;
#863 = DIRECTION ( 'NONE',  ( 0.000000000000000000, 0.000000000000000000, 1.000000000000000000 ) ) ;
#864 = ORIENTED_EDGE ( 'NONE', *, *, #1314, .T. ) ;
#865 = CARTESIAN_POINT ( 'NONE',  ( -145.0000000000000284, 2.993649167310367343, 45.00000000000000000 ) ) ;
#866 = AXIS2_PLACEMENT_3D ( 'NONE', #2099, #740, #924 ) ;
#867 = DIRECTION ( 'NONE',  ( 0.000000000000000000, 0.000000000000000000, 1.000000000000000000 ) ) ;
#868 = EDGE_CURVE ( 'NONE', #749, #94, #532, .T. ) ;
#869 = ADVANCED_FACE ( 'NONE', ( #1116 ), #565, .F. ) ;
#870 = ORIENTED_EDGE ( 'NONE', *, *, #1956, .F. ) ;
#871 = EDGE_LOOP ( 'NONE', ( #488, #1641, #432, #921, #1341, #790 ) ) ;
#872 = DIRECTION ( 'NONE',  ( 6.123233995736766036E-17, -1.000000000000000000, 0.000000000000000000 ) ) ;
#873 = CARTESIAN_POINT ( 'NONE',  ( 2.500000000000000000, -2.357898499370432166, 3.035766082959412415E-15 ) ) ;
#874 = AXIS2_PLACEMENT_3D ( 'NONE', #1863, #331, #2 ) ;
#875 = AXIS2_PLACEMENT_3D ( 'NONE', #2226, #542, #211 ) ;
#876 = AXIS2_PLACEMENT_3D ( 'NONE', #1434, #2120, #1782 ) ;
#877 = DIRECTION ( 'NONE',  ( 1.000000000000000000, 6.123233995736766036E-17, -1.224646799147353207E-16 ) ) ;
#878 = VECTOR ( 'NONE', #1632, 1000.000000000000000 ) ;
#879 = EDGE_CURVE ( 'NONE', #1097, #463, #2057, .T. ) ;
#880 = EDGE_CURVE ( 'NONE', #1358, #463, #576, .T. ) ;
#881 = ORIENTED_EDGE ( 'NONE', *, *, #224, .T. ) ;
#882 = CARTESIAN_POINT ( 'NONE',  ( -157.0000000000000000, 10.00000000000000000, -56.99999999999997868 ) ) ;
#883 = DIRECTION ( 'NONE',  ( 0.000000000000000000, 0.000000000000000000, 1.000000000000000000 ) ) ;
#884 = DIRECTION ( 'NONE',  ( -1.000000000000000000, -0.000000000000000000, -0.000000000000000000 ) ) ;
#885 = AXIS2_PLACEMENT_3D ( 'NONE', #1917, #892, #1378 ) ;
#886 = DIRECTION ( 'NONE',  ( 2.312964634635742957E-16, 0.000000000000000000, -1.000000000000000000 ) ) ;
#887 = DIRECTION ( 'NONE',  ( 0.000000000000000000, 0.000000000000000000, 1.000000000000000000 ) ) ;
#888 = APPLICATION_CONTEXT ( 'automotive_design' ) ;
#889 = CIRCLE ( 'NONE', #2219, 2.649999999999985700 ) ;
#890 = ORIENTED_EDGE ( 'NONE', *, *, #165, .T. ) ;
#891 = CARTESIAN_POINT ( 'NONE',  ( 2.500000000000000000, 2.500728763858895382E-16, -2.041999999999999815 ) ) ;
#892 = DIRECTION ( 'NONE',  ( -0.000000000000000000, 1.000000000000000000, -0.000000000000000000 ) ) ;
#893 = DIRECTION ( 'NONE',  ( -0.000000000000000000, -1.000000000000000000, -0.000000000000000000 ) ) ;
#894 = CARTESIAN_POINT ( 'NONE',  ( 2.500000000000000000, 2.357898499370431722, -2.818925648462311528E-15 ) ) ;
#895 = CIRCLE ( 'NONE', #327, 2.041999999999999815 ) ;
#896 = LINE ( 'NONE', #21, #2199 ) ;
#897 = PRESENTATION_STYLE_ASSIGNMENT (( #1400 ) ) ;
#898 = VERTEX_POINT ( 'NONE', #1249 ) ;
#899 = VERTEX_POINT ( 'NONE', #1130 ) ;
#900 = DIRECTION ( 'NONE',  ( 0.000000000000000000, 0.000000000000000000, 1.000000000000000000 ) ) ;
#901 = CARTESIAN_POINT ( 'NONE',  ( -139.9999999999999716, -120.0000000000000142, 50.00000000000000000 ) ) ;
#902 = DIRECTION ( 'NONE',  ( 6.123233995736766036E-17, -1.000000000000000000, 0.000000000000000000 ) ) ;
#903 = EDGE_CURVE ( 'NONE', #1057, #2205, #422, .T. ) ;
#904 = DIRECTION ( 'NONE',  ( 6.123233995736766036E-17, -1.000000000000000000, 0.000000000000000000 ) ) ;
#905 = PRESENTATION_LAYER_ASSIGNMENT (  '', '', ( #1549 ) ) ;
#906 = VECTOR ( 'NONE', #29, 1000.000000000000000 ) ;
#907 = VECTOR ( 'NONE', #1714, 1000.000000000000000 ) ;
#908 = CARTESIAN_POINT ( 'NONE',  ( 2.500000000000000000, 2.357898499370431722, -2.818925648462311528E-15 ) ) ;
#909 = ORIENTED_EDGE ( 'NONE', *, *, #966, .T. ) ;
#910 = EDGE_CURVE ( 'NONE', #1188, #267, #693, .T. ) ;
#911 = ORIENTED_EDGE ( 'NONE', *, *, #1571, .F. ) ;
#912 = CARTESIAN_POINT ( 'NONE',  ( 0.000000000000000000, 0.000000000000000000, 0.000000000000000000 ) ) ;
#913 = FACE_BOUND ( 'NONE', #379, .T. ) ;
#914 = EDGE_CURVE ( 'NONE', #256, #848, #1946, .T. ) ;
#915 = ORIENTED_EDGE ( 'NONE', *, *, #40, .F. ) ;
#916 = FILL_AREA_STYLE ('',( #221 ) ) ;
#917 = ADVANCED_FACE ( 'NONE', ( #87 ), #1301, .F. ) ;
#918 = DIRECTION ( 'NONE',  ( 0.000000000000000000, 0.000000000000000000, 1.000000000000000000 ) ) ;
#919 = CARTESIAN_POINT ( 'NONE',  ( 145.0000000000000284, 2.800000000000000266, -47.70000000000000284 ) ) ;
#920 = CIRCLE ( 'NONE', #1173, 2.041999999999999815 ) ;
#921 = ORIENTED_EDGE ( 'NONE', *, *, #1077, .T. ) ;
#922 = ORIENTED_EDGE ( 'NONE', *, *, #522, .F. ) ;
#923 = DIRECTION ( 'NONE',  ( 0.000000000000000000, 0.000000000000000000, 1.000000000000000000 ) ) ;
#924 = DIRECTION ( 'NONE',  ( 0.000000000000000000, 0.000000000000000000, 1.000000000000000000 ) ) ;
#925 = CYLINDRICAL_SURFACE ( 'NONE', #1837, 2.500000000000002220 ) ;
#926 = VECTOR ( 'NONE', #551, 1000.000000000000000 ) ;
#927 = VECTOR ( 'NONE', #1972, 1000.000000000000000 ) ;
#928 = CARTESIAN_POINT ( 'NONE',  ( -145.0000000000000284, -15.00000000000003197, -45.00000000000000000 ) ) ;
#929 = EDGE_CURVE ( 'NONE', #1700, #44, #963, .T. ) ;
#930 = EDGE_LOOP ( 'NONE', ( #1413, #1074 ) ) ;
#931 = EDGE_CURVE ( 'NONE', #166, #396, #2202, .T. ) ;
#932 =( GEOMETRIC_REPRESENTATION_CONTEXT ( 3 ) GLOBAL_UNCERTAINTY_ASSIGNED_CONTEXT ( ( #502 ) ) GLOBAL_UNIT_ASSIGNED_CONTEXT ( ( #1094, #1389, #1217 ) ) REPRESENTATION_CONTEXT ( 'NONE', 'WORKASPACE' ) );
#933 = EDGE_LOOP ( 'NONE', ( #584, #861, #1975, #1295 ) ) ;
#934 = LINE ( 'NONE', #2131, #397 ) ;
#935 = DIRECTION ( 'NONE',  ( 0.000000000000000000, -1.000000000000000000, 1.287488025362403787E-15 ) ) ;
#937 = EDGE_LOOP ( 'NONE', ( #1629, #1796 ) ) ;
#936 = DIRECTION ( 'NONE',  ( 6.123233995736766036E-17, -1.000000000000000000, 0.000000000000000000 ) ) ;
#938 = PLANE ( 'NONE',  #1932 ) ;
#939 = LINE ( 'NONE', #758, #680 ) ;
#940 = PRODUCT_DEFINITION_FORMATION_WITH_SPECIFIED_SOURCE ( 'ANY', '', #72, .NOT_KNOWN. ) ;
#941 = ADVANCED_FACE ( 'NONE', ( #1982 ), #733, .F. ) ;
#942 = CIRCLE ( 'NONE', #441, 2.700000000000001066 ) ;
#943 = PRODUCT_CONTEXT ( 'NONE', #2073, 'mechanical' ) ;
#944 = TOROIDAL_SURFACE ( 'NONE', #1407, 2.700000000000000622, 0.2000000000000000111 ) ;
#945 = ORIENTED_EDGE ( 'NONE', *, *, #1314, .F. ) ;
#946 = ADVANCED_FACE ( 'NONE', ( #1091 ), #1514, .T. ) ;
#947 = ORIENTED_EDGE ( 'NONE', *, *, #903, .T. ) ;
#948 = LINE ( 'NONE', #37, #1541 ) ;
#949 = CARTESIAN_POINT ( 'NONE',  ( -145.0000000000000284, -3.353798720221824946E-14, 45.00000000000000000 ) ) ;
#950 = EDGE_LOOP ( 'NONE', ( #973, #1636 ) ) ;
#952 = ORIENTED_EDGE ( 'NONE', *, *, #1176, .F. ) ;
#951 = DIRECTION ( 'NONE',  ( -0.000000000000000000, -0.000000000000000000, -1.000000000000000000 ) ) ;
#953 = DIRECTION ( 'NONE',  ( -2.312964634635742957E-16, -0.000000000000000000, 1.000000000000000000 ) ) ;
#954 = CARTESIAN_POINT ( 'NONE',  ( 145.0000000000000284, 3.000000000000000000, -47.64999999999998437 ) ) ;
#955 = CONTEXT_DEPENDENT_SHAPE_REPRESENTATION ( #1847, #1820 ) ;
#956 = EDGE_LOOP ( 'NONE', ( #158, #827, #204, #1550 ) ) ;
#957 = VERTEX_POINT ( 'NONE', #1418 ) ;
#958 = PLANE ( 'NONE',  #1828 ) ;
#959 = CARTESIAN_POINT ( 'NONE',  ( 4.999999999999997335, 5.204748896376250699E-16, -4.250000000000000000 ) ) ;
#960 = ORIENTED_EDGE ( 'NONE', *, *, #1077, .F. ) ;
#962 = ORIENTED_EDGE ( 'NONE', *, *, #1762, .F. ) ;
#961 = DIRECTION ( 'NONE',  ( 0.000000000000000000, 0.000000000000000000, -1.000000000000000000 ) ) ;
#963 = LINE ( 'NONE', #1645, #1693 ) ;
#964 = APPLICATION_CONTEXT ( 'automotive_design' ) ;
#965 = CIRCLE ( 'NONE', #391, 2.700000000000000622 ) ;
#966 = EDGE_CURVE ( 'NONE', #1672, #80, #254, .T. ) ;
#967 = PRODUCT ( 'socket head cap screw_iso_ISO 4762 M5 x 16 - 16N', 'socket head cap screw_iso_ISO 4762 M5 x 16 - 16N', '', ( #773 ) ) ;
#968 = FACE_BOUND ( 'NONE', #937, .T. ) ;
#969 = MANIFOLD_SOLID_BREP ( 'Cavity1', #2111 ) ;
#970 = SHAPE_DEFINITION_REPRESENTATION ( #425, #354 ) ;
#971 = CARTESIAN_POINT ( 'NONE',  ( 0.000000000000000000, 0.000000000000000000, 0.000000000000000000 ) ) ;
#972 =( GEOMETRIC_REPRESENTATION_CONTEXT ( 3 ) GLOBAL_UNCERTAINTY_ASSIGNED_CONTEXT ( ( #1529 ) ) GLOBAL_UNIT_ASSIGNED_CONTEXT ( ( #1311, #1997, #460 ) ) REPRESENTATION_CONTEXT ( 'NONE', 'WORKASPACE' ) );
#973 = ORIENTED_EDGE ( 'NONE', *, *, #1363, .F. ) ;
#974 = CARTESIAN_POINT ( 'NONE',  ( 21.00000000000000355, 2.516649172247811061E-16, -2.055000000000000160 ) ) ;
#975 = ORIENTED_EDGE ( 'NONE', *, *, #1973, .T. ) ;
#976 = AXIS2_PLACEMENT_3D ( 'NONE', #807, #479, #1345 ) ;
#977 = AXIS2_PLACEMENT_3D ( 'NONE', #105, #798, #1765 ) ;
#978 = FACE_OUTER_BOUND ( 'NONE', #956, .T. ) ;
#979 = ADVANCED_FACE ( 'NONE', ( #1010 ), #804, .F. ) ;
#980 = DIRECTION ( 'NONE',  ( 6.123233995736766036E-17, -1.000000000000000000, 0.000000000000000000 ) ) ;
#981 = DIRECTION ( 'NONE',  ( 0.000000000000000000, -1.000000000000000000, 0.000000000000000000 ) ) ;
#982 = PLANE ( 'NONE',  #395 ) ;
#983 = SHAPE_REPRESENTATION_RELATIONSHIP ( 'NONE' , 'NONE' ,  #261, #2138 ) ;
#984 = AXIS2_PLACEMENT_3D ( 'NONE', #1496, #981, #1678 ) ;
#985 = ORIENTED_EDGE ( 'NONE', *, *, #1312, .F. ) ;
#986 = AXIS2_PLACEMENT_3D ( 'NONE', #2080, #877, #1388 ) ;
#987 = ORIENTED_EDGE ( 'NONE', *, *, #559, .T. ) ;
#988 = EDGE_CURVE ( 'NONE', #2205, #1883, #127, .T. ) ;
#989 = LINE ( 'NONE', #1174, #506 ) ;
#990 = DIRECTION ( 'NONE',  ( -1.000000000000000000, -0.000000000000000000, -0.000000000000000000 ) ) ;
#991 = CARTESIAN_POINT ( 'NONE',  ( -145.0000000000000284, -3.358697307418414604E-14, 47.50000000000000000 ) ) ;
#992 = DIRECTION ( 'NONE',  ( 0.000000000000000000, 1.000000000000000000, -1.287488025362403787E-15 ) ) ;
#993 = EDGE_CURVE ( 'NONE', #80, #1672, #1984, .T. ) ;
#994 = ORIENTED_EDGE ( 'NONE', *, *, #1992, .T. ) ;
#995 = DIRECTION ( 'NONE',  ( -1.000000000000000000, 0.000000000000000000, -2.312964634635742957E-16 ) ) ;
#996 = ORIENTED_EDGE ( 'NONE', *, *, #1197, .F. ) ;
#997 = CIRCLE ( 'NONE', #594, 2.649999999999985700 ) ;
#998 = DIRECTION ( 'NONE',  ( 1.000000000000000000, 0.000000000000000000, 0.000000000000000000 ) ) ;
#999 = DIRECTION ( 'NONE',  ( -1.000000000000000000, -0.000000000000000000, -0.000000000000000000 ) ) ;
#1000 = ORIENTED_EDGE ( 'NONE', *, *, #1331, .T. ) ;
#1001 = DIRECTION ( 'NONE',  ( 1.000000000000000000, 0.000000000000000000, 0.000000000000000000 ) ) ;
#1002 = DIRECTION ( 'NONE',  ( -1.000000000000000000, 0.000000000000000000, 4.336808689942017736E-17 ) ) ;
#1003 = PRODUCT_DEFINITION_CONTEXT ( 'detailed design', #964, 'design' ) ;
#1004 = ORIENTED_EDGE ( 'NONE', *, *, #1712, .F. ) ;
#1005 = AXIS2_PLACEMENT_3D ( 'NONE', #2215, #1350, #663 ) ;
#1006 = DIRECTION ( 'NONE',  ( 0.000000000000000000, 0.000000000000000000, -1.000000000000000000 ) ) ;
#1007 = EDGE_CURVE ( 'NONE', #2053, #776, #1376, .T. ) ;
#1008 = ORIENTED_EDGE ( 'NONE', *, *, #966, .F. ) ;
#1009 = CARTESIAN_POINT ( 'NONE',  ( 157.0000000000000000, 3.000000000000000000, -56.99999999999999289 ) ) ;
#1010 = FACE_OUTER_BOUND ( 'NONE', #2135, .T. ) ;
#1011 = AXIS2_PLACEMENT_3D ( 'NONE', #275, #62, #1082 ) ;
#1012 = EDGE_LOOP ( 'NONE', ( #1706, #1747, #125 ) ) ;
#1013 = DIRECTION ( 'NONE',  ( -0.000000000000000000, 1.000000000000000000, -0.000000000000000000 ) ) ;
#1014 = DIRECTION ( 'NONE',  ( -0.000000000000000000, -0.000000000000000000, 1.000000000000000000 ) ) ;
#1015 = EDGE_LOOP ( 'NONE', ( #960, #796, #2059, #84, #1520 ) ) ;
#1016 = ADVANCED_FACE ( 'NONE', ( #1845 ), #1676, .F. ) ;
#1017 = ORIENTED_EDGE ( 'NONE', *, *, #2177, .T. ) ;
#1018 =( GEOMETRIC_REPRESENTATION_CONTEXT ( 3 ) GLOBAL_UNCERTAINTY_ASSIGNED_CONTEXT ( ( #1357 ) ) GLOBAL_UNIT_ASSIGNED_CONTEXT ( ( #618, #664, #2203 ) ) REPRESENTATION_CONTEXT ( 'NONE', 'WORKASPACE' ) );
#1019 = VECTOR ( 'NONE', #1025, 1000.000000000000000 ) ;
#1020 = DIRECTION ( 'NONE',  ( -1.000000000000000000, -0.000000000000000000, -0.000000000000000000 ) ) ;
#1021 = AXIS2_PLACEMENT_3D ( 'NONE', #1953, #2146, #1247 ) ;
#1022 = FACE_OUTER_BOUND ( 'NONE', #497, .T. ) ;
#1023 = PRODUCT_DEFINITION_CONTEXT ( 'detailed design', #888, 'design' ) ;
#1024 = ORIENTED_EDGE ( 'NONE', *, *, #988, .F. ) ;
#1025 = DIRECTION ( 'NONE',  ( -0.000000000000000000, 1.000000000000000000, -0.000000000000000000 ) ) ;
#1026 = DIRECTION ( 'NONE',  ( -1.000000000000000000, -0.000000000000000000, -0.000000000000000000 ) ) ;
#1027 = DIRECTION ( 'NONE',  ( 1.000000000000000000, 0.000000000000000000, 0.000000000000000000 ) ) ;
#1028 = ORIENTED_EDGE ( 'NONE', *, *, #2194, .F. ) ;
#1029 = ORIENTED_EDGE ( 'NONE', *, *, #232, .T. ) ;
#1030 = DIRECTION ( 'NONE',  ( 1.049727191138618696E-16, 0.5150380749100541555, -0.8571673007021122226 ) ) ;
#1031 = PLANE ( 'NONE',  #1955 ) ;
#1032 = ORIENTED_EDGE ( 'NONE', *, *, #224, .F. ) ;
#1033 = DIRECTION ( 'NONE',  ( -1.000000000000000000, -0.000000000000000000, -0.000000000000000000 ) ) ;
#1034 = EDGE_CURVE ( 'NONE', #1579, #4, #1224, .T. ) ;
#1035 =( NAMED_UNIT ( * ) PLANE_ANGLE_UNIT ( ) SI_UNIT ( $, .RADIAN. ) );
#1036 = VECTOR ( 'NONE', #1591, 1000.000000000000000 ) ;
#1037 = EDGE_LOOP ( 'NONE', ( #523, #987, #2096, #1277 ) ) ;
#1038 = ORIENTED_EDGE ( 'NONE', *, *, #2124, .T. ) ;
#1039 = DIRECTION ( 'NONE',  ( 0.000000000000000000, 0.000000000000000000, 1.000000000000000000 ) ) ;
#1040 = CARTESIAN_POINT ( 'NONE',  ( -160.0000000000000284, 10.00000000000000000, 60.00000000000001421 ) ) ;
#1041 = CARTESIAN_POINT ( 'NONE',  ( -145.0000000000000284, 3.000000000000000000, -47.64999999999998437 ) ) ;
#1042 = ADVANCED_FACE ( 'NONE', ( #829 ), #1175, .F. ) ;
#1043 = VECTOR ( 'NONE', #1912, 1000.000000000000000 ) ;
#1044 = DIRECTION ( 'NONE',  ( 0.000000000000000000, 0.000000000000000000, 1.000000000000000000 ) ) ;
#1045 =( REPRESENTATION_RELATIONSHIP ('NONE','NONE', #367, #38 ) REPRESENTATION_RELATIONSHIP_WITH_TRANSFORMATION ( #1325 )SHAPE_REPRESENTATION_RELATIONSHIP( ) );
#1046 = ORIENTED_EDGE ( 'NONE', *, *, #1900, .T. ) ;
#1047 = DIRECTION ( 'NONE',  ( 0.000000000000000000, -1.000000000000000000, 0.000000000000000000 ) ) ;
#1048 = CARTESIAN_POINT ( 'NONE',  ( -157.0000000000000000, 3.000000000000000000, -3.631354476378115974E-14 ) ) ;
#1049 =( GEOMETRIC_REPRESENTATION_CONTEXT ( 3 ) GLOBAL_UNCERTAINTY_ASSIGNED_CONTEXT ( ( #348 ) ) GLOBAL_UNIT_ASSIGNED_CONTEXT ( ( #93, #307, #812 ) ) REPRESENTATION_CONTEXT ( 'NONE', 'WORKASPACE' ) );
#1050 = AXIS2_PLACEMENT_3D ( 'NONE', #163, #662, #2200 ) ;
#1051 = VECTOR ( 'NONE', #1467, 1000.000000000000114 ) ;
#1052 = DIRECTION ( 'NONE',  ( 0.000000000000000000, 0.000000000000000000, 1.000000000000000000 ) ) ;
#1053 = ORIENTED_EDGE ( 'NONE', *, *, #1547, .F. ) ;
#1054 = LINE ( 'NONE', #689, #168 ) ;
#1055 = CARTESIAN_POINT ( 'NONE',  ( 145.0000000000000284, 2.993649167310367343, 42.35000000000001563 ) ) ;
#1056 = CARTESIAN_POINT ( 'NONE',  ( -139.9999999999999716, -120.0000000000000142, -50.00000000000000000 ) ) ;
#1057 = VERTEX_POINT ( 'NONE', #2006 ) ;
#1058 = CARTESIAN_POINT ( 'NONE',  ( -150.0000000000000284, -9.999999999999994671, -40.00000000000000000 ) ) ;
#1059 = VECTOR ( 'NONE', #2062, 1000.000000000000000 ) ;
#1060 = CARTESIAN_POINT ( 'NONE',  ( 159.9999999999999716, 0.000000000000000000, 60.00000000000001421 ) ) ;
#1061 = FACE_OUTER_BOUND ( 'NONE', #343, .T. ) ;
#1062 = ADVANCED_FACE ( 'NONE', ( #637 ), #493, .T. ) ;
#1063 = VECTOR ( 'NONE', #288, 999.9999999999997726 ) ;
#1064 = ORIENTED_EDGE ( 'NONE', *, *, #1150, .T. ) ;
#1065 = ORIENTED_EDGE ( 'NONE', *, *, #586, .F. ) ;
#1066 = CARTESIAN_POINT ( 'NONE',  ( -145.0000000000000284, 2.800000000000000266, -45.00000000000000000 ) ) ;
#1067 = DIRECTION ( 'NONE',  ( 0.000000000000000000, -0.4999999999999993339, 0.8660254037844390407 ) ) ;
#1068 = DIRECTION ( 'NONE',  ( -0.000000000000000000, 0.000000000000000000, -1.000000000000000000 ) ) ;
#1069 = CARTESIAN_POINT ( 'NONE',  ( 2.500000000000000000, -1.768423874527825568, -1.020999999999998575 ) ) ;
#1070 = CIRCLE ( 'NONE', #1365, 2.700000000000001066 ) ;
#1071 = CARTESIAN_POINT ( 'NONE',  ( -139.9999999999999716, 2.312964634635743056E-15, 50.00000000000000000 ) ) ;
#1072 = LINE ( 'NONE', #1901, #1043 ) ;
#1073 = AXIS2_PLACEMENT_3D ( 'NONE', #1698, #998, #1675 ) ;
#1074 = ORIENTED_EDGE ( 'NONE', *, *, #1134, .F. ) ;
#1075 = EDGE_CURVE ( 'NONE', #1159, #2218, #227, .T. ) ;
#1076 = ORIENTED_EDGE ( 'NONE', *, *, #1588, .T. ) ;
#1077 = EDGE_CURVE ( 'NONE', #537, #847, #1858, .T. ) ;
#1078 = LINE ( 'NONE', #901, #794 ) ;
#1079 = DIRECTION ( 'NONE',  ( 0.000000000000000000, 0.000000000000000000, 1.000000000000000000 ) ) ;
#1080 = DIRECTION ( 'NONE',  ( 0.000000000000000000, 1.000000000000000000, -1.287488025362403787E-15 ) ) ;
#1081 = AXIS2_PLACEMENT_3D ( 'NONE', #362, #2055, #1027 ) ;
#1082 = DIRECTION ( 'NONE',  ( -1.000000000000000000, 0.000000000000000000, 0.000000000000000000 ) ) ;
#1083 = AXIS2_PLACEMENT_3D ( 'NONE', #273, #1931, #1773 ) ;
#1084 = DIRECTION ( 'NONE',  ( -0.000000000000000000, 1.000000000000000000, -0.000000000000000000 ) ) ;
#1085 = APPLICATION_CONTEXT ( 'automotive_design' ) ;
#1086 = ORIENTED_EDGE ( 'NONE', *, *, #645, .F. ) ;
#1087 = ORIENTED_EDGE ( 'NONE', *, *, #1145, .T. ) ;
#1088 = DIRECTION ( 'NONE',  ( 0.000000000000000000, -1.224646799147353454E-16, 1.000000000000000000 ) ) ;
#1089 = FACE_OUTER_BOUND ( 'NONE', #2035, .T. ) ;
#1090 = CARTESIAN_POINT ( 'NONE',  ( -145.0000000000000284, 2.800000000000000266, 45.00000000000000000 ) ) ;
#1091 = FACE_OUTER_BOUND ( 'NONE', #1682, .T. ) ;
#1092 = EDGE_CURVE ( 'NONE', #1188, #1663, #1635, .T. ) ;
#1093 = CARTESIAN_POINT ( 'NONE',  ( 0.000000000000000000, 0.000000000000000000, 0.000000000000000000 ) ) ;
#1094 =( LENGTH_UNIT ( ) NAMED_UNIT ( * ) SI_UNIT ( .MILLI., .METRE. ) );
#1095 = EDGE_CURVE ( 'NONE', #2156, #1057, #1508, .T. ) ;
#1096 = VECTOR ( 'NONE', #763, 1000.000000000000000 ) ;
#1097 = VERTEX_POINT ( 'NONE', #1833 ) ;
#1098 = ORIENTED_EDGE ( 'NONE', *, *, #670, .F. ) ;
#1099 = CARTESIAN_POINT ( 'NONE',  ( 0.2500000000000002220, 4.898587196589412829E-16, -4.000000000000000000 ) ) ;
#1100 = DIRECTION ( 'NONE',  ( -1.000000000000000000, -0.000000000000000000, 4.336808689942017736E-17 ) ) ;
#1101 = CARTESIAN_POINT ( 'NONE',  ( 2.500000000000000000, -1.178949249685214307, 2.042000000000001592 ) ) ;
#1102 = ORIENTED_EDGE ( 'NONE', *, *, #306, .F. ) ;
#1103 = EDGE_CURVE ( 'NONE', #830, #2053, #920, .T. ) ;
#1104 = CARTESIAN_POINT ( 'NONE',  ( -149.9999999999999716, -120.0000000000000142, 40.00000000000000000 ) ) ;
#1105 = AXIS2_PLACEMENT_3D ( 'NONE', #1958, #1786, #1623 ) ;
#1106 = LINE ( 'NONE', #1785, #927 ) ;
#1107 = ADVANCED_FACE ( 'NONE', ( #1022 ), #1688, .T. ) ;
#1108 = CARTESIAN_POINT ( 'NONE',  ( 0.000000000000000000, 0.000000000000000000, 0.000000000000000000 ) ) ;
#1109 = FILL_AREA_STYLE ('',( #1814 ) ) ;
#1110 = EDGE_LOOP ( 'NONE', ( #2079, #2004, #1371, #792 ) ) ;
#1111 = ORIENTED_EDGE ( 'NONE', *, *, #135, .F. ) ;
#1112 = PLANE ( 'NONE',  #1894 ) ;
#1113 = FACE_BOUND ( 'NONE', #351, .T. ) ;
#1115 = ORIENTED_EDGE ( 'NONE', *, *, #1181, .T. ) ;
#1114 = DIRECTION ( 'NONE',  ( -1.000000000000000000, 0.000000000000000000, -2.312964634635742957E-16 ) ) ;
#1116 = FACE_OUTER_BOUND ( 'NONE', #622, .T. ) ;
#1117 = FACE_OUTER_BOUND ( 'NONE', #2025, .T. ) ;
#1118 = DIRECTION ( 'NONE',  ( -1.000000000000000000, -0.000000000000000000, -0.000000000000000000 ) ) ;
#1119 = STYLED_ITEM ( 'NONE', ( #2188 ), #2138 ) ;
#1120 = VECTOR ( 'NONE', #884, 1000.000000000000000 ) ;
#1121 = CONTEXT_DEPENDENT_SHAPE_REPRESENTATION ( #2036, #1282 ) ;
#1122 = AXIS2_PLACEMENT_3D ( 'NONE', #1784, #2151, #784 ) ;
#1123 = AXIS2_PLACEMENT_3D ( 'NONE', #230, #1750, #1628 ) ;
#1124 = ORIENTED_EDGE ( 'NONE', *, *, #378, .T. ) ;
#1125 = VERTEX_POINT ( 'NONE', #1471 ) ;
#1126 = CARTESIAN_POINT ( 'NONE',  ( 0.000000000000000000, 0.000000000000000000, -40.00000000000000000 ) ) ;
#1127 = ORIENTED_EDGE ( 'NONE', *, *, #1923, .T. ) ;
#1129 = ORIENTED_EDGE ( 'NONE', *, *, #684, .T. ) ;
#1128 = FACE_OUTER_BOUND ( 'NONE', #172, .T. ) ;
#1130 = CARTESIAN_POINT ( 'NONE',  ( -145.0000000000000284, -15.00000000000003197, -47.50000000000000000 ) ) ;
#1131 = DIRECTION ( 'NONE',  ( 0.000000000000000000, 0.000000000000000000, -1.000000000000000000 ) ) ;
#1132 = FACE_OUTER_BOUND ( 'NONE', #1268, .T. ) ;
#1133 = VERTEX_POINT ( 'NONE', #1332 ) ;
#1134 = EDGE_CURVE ( 'NONE', #625, #671, #194, .T. ) ;
#1135 = ORIENTED_EDGE ( 'NONE', *, *, #1788, .F. ) ;
#1136 = DIRECTION ( 'NONE',  ( 1.000000000000000000, -0.000000000000000000, 2.312964634635742957E-16 ) ) ;
#1137 = EDGE_LOOP ( 'NONE', ( #1401, #1289, #2074, #456 ) ) ;
#1138 = CARTESIAN_POINT ( 'NONE',  ( 2.500000000000000000, -1.178949249685214307, 2.042000000000001592 ) ) ;
#1139 = VECTOR ( 'NONE', #258, 1000.000000000000000 ) ;
#1140 = FACE_OUTER_BOUND ( 'NONE', #1617, .T. ) ;
#1141 = FACE_OUTER_BOUND ( 'NONE', #676, .T. ) ;
#1142 = ITEM_DEFINED_TRANSFORMATION ( 'NONE', 'NONE', #874,  #30 ) ;
#1143 = EDGE_CURVE ( 'NONE', #220, #1831, #628, .T. ) ;
#1144 = ORIENTED_EDGE ( 'NONE', *, *, #914, .F. ) ;
#1145 = EDGE_CURVE ( 'NONE', #1444, #216, #701, .T. ) ;
#1146 = CARTESIAN_POINT ( 'NONE',  ( -145.0000000000000284, 3.000000000000000000, -45.00000000000000000 ) ) ;
#1147 = ORIENTED_EDGE ( 'NONE', *, *, #509, .F. ) ;
#1148 = AXIS2_PLACEMENT_3D ( 'NONE', #126, #499, #678 ) ;
#1149 = AXIS2_PLACEMENT_3D ( 'NONE', #1454, #420, #1270 ) ;
#1150 = EDGE_CURVE ( 'NONE', #1509, #1133, #2069, .T. ) ;
#1151 = DIRECTION ( 'NONE',  ( 1.000000000000000000, 0.000000000000000000, 0.000000000000000000 ) ) ;
#1152 = DIRECTION ( 'NONE',  ( -1.000000000000000000, 0.000000000000000000, 0.000000000000000000 ) ) ;
#1153 = CARTESIAN_POINT ( 'NONE',  ( -145.0000000000000284, -3.358697307418414604E-14, -45.00000000000000000 ) ) ;
#1154 = DIRECTION ( 'NONE',  ( 0.000000000000000000, 0.000000000000000000, -1.000000000000000000 ) ) ;
#1155 = SHAPE_DEFINITION_REPRESENTATION ( #1621, #38 ) ;
#1156 =( GEOMETRIC_REPRESENTATION_CONTEXT ( 3 ) GLOBAL_UNCERTAINTY_ASSIGNED_CONTEXT ( ( #2211 ) ) GLOBAL_UNIT_ASSIGNED_CONTEXT ( ( #247, #1487, #472 ) ) REPRESENTATION_CONTEXT ( 'NONE', 'WORKASPACE' ) );
#1157 = CIRCLE ( 'NONE', #183, 2.055000000000000160 ) ;
#1158 = VECTOR ( 'NONE', #791, 1000.000000000000000 ) ;
#1159 = VERTEX_POINT ( 'NONE', #160 ) ;
#1160 = DIRECTION ( 'NONE',  ( 1.049727191138618696E-16, 0.5150380749100541555, -0.8571673007021122226 ) ) ;
#1161 = AXIS2_PLACEMENT_3D ( 'NONE', #312, #1164, #2210 ) ;
#1162 = ORIENTED_EDGE ( 'NONE', *, *, #208, .T. ) ;
#1163 = PLANE ( 'NONE',  #1540 ) ;
#1164 = DIRECTION ( 'NONE',  ( -1.000000000000000000, -0.000000000000000000, -0.000000000000000000 ) ) ;
#1165 = VERTEX_POINT ( 'NONE', #1404 ) ;
#1166 = DIRECTION ( 'NONE',  ( -0.000000000000000000, -1.000000000000000000, -0.000000000000000000 ) ) ;
#1167 = DIRECTION ( 'NONE',  ( 1.000000000000000000, 0.000000000000000000, 0.000000000000000000 ) ) ;
#1168 = EDGE_CURVE ( 'NONE', #463, #1097, #316, .T. ) ;
#1169 = EDGE_CURVE ( 'NONE', #1509, #1284, #376, .T. ) ;
#1170 = EDGE_LOOP ( 'NONE', ( #1976, #1493, #167, #592 ) ) ;
#1171 = CARTESIAN_POINT ( 'NONE',  ( -150.0000000000000284, -9.999999999999994671, -40.00000000000000000 ) ) ;
#1172 = ORIENTED_EDGE ( 'NONE', *, *, #520, .F. ) ;
#1173 = AXIS2_PLACEMENT_3D ( 'NONE', #301, #990, #649 ) ;
#1174 = CARTESIAN_POINT ( 'NONE',  ( -145.0000000000000284, -15.00000000000003197, 47.50000000000000000 ) ) ;
#1175 = CYLINDRICAL_SURFACE ( 'NONE', #155, 2.500000000000002220 ) ;
#1176 = EDGE_CURVE ( 'NONE', #1421, #833, #1907, .T. ) ;
#1177 = ORIENTED_EDGE ( 'NONE', *, *, #384, .F. ) ;
#1178 = DIRECTION ( 'NONE',  ( 0.000000000000000000, 0.000000000000000000, -1.000000000000000000 ) ) ;
#1179 = AXIS2_PLACEMENT_3D ( 'NONE', #1881, #1888, #900 ) ;
#1180 = FACE_OUTER_BOUND ( 'NONE', #398, .T. ) ;
#1181 = EDGE_CURVE ( 'NONE', #671, #625, #1387, .T. ) ;
#1182 =( NAMED_UNIT ( * ) SI_UNIT ( $, .STERADIAN. ) SOLID_ANGLE_UNIT ( ) );
#1183 = ORIENTED_EDGE ( 'NONE', *, *, #1573, .T. ) ;
#1184 = VECTOR ( 'NONE', #787, 1000.000000000000000 ) ;
#1185 = EDGE_LOOP ( 'NONE', ( #1512, #1326, #2170, #598 ) ) ;
#1186 = DIRECTION ( 'NONE',  ( 2.312964634635742957E-16, -1.000000000000000000, 0.000000000000000000 ) ) ;
#1187 = CARTESIAN_POINT ( 'NONE',  ( 5.200000000000002842, 0.000000000000000000, 0.000000000000000000 ) ) ;
#1188 = VERTEX_POINT ( 'NONE', #1055 ) ;
#1189 = DIRECTION ( 'NONE',  ( -6.123233995736766036E-17, 1.000000000000000000, -0.000000000000000000 ) ) ;
#1190 = DIRECTION ( 'NONE',  ( 1.000000000000000000, 6.123233995736766036E-17, -1.224646799147353207E-16 ) ) ;
#1191 = DIRECTION ( 'NONE',  ( 6.123233995736766036E-17, -1.000000000000000000, 0.000000000000000000 ) ) ;
#1192 = ORIENTED_EDGE ( 'NONE', *, *, #781, .T. ) ;
#1193 = ORIENTED_EDGE ( 'NONE', *, *, #1542, .T. ) ;
#1194 = CIRCLE ( 'NONE', #1983, 2.649999999999985700 ) ;
#1195 = VECTOR ( 'NONE', #1891, 1000.000000000000000 ) ;
#1196 = CARTESIAN_POINT ( 'NONE',  ( 145.0000000000000284, 2.800000000000000266, -45.00000000000000000 ) ) ;
#1197 = EDGE_CURVE ( 'NONE', #653, #694, #2090, .T. ) ;
#1198 = FACE_OUTER_BOUND ( 'NONE', #411, .T. ) ;
#1199 = PRODUCT_DEFINITION_CONTEXT ( 'detailed design', #1501, 'design' ) ;
#1200 = EDGE_LOOP ( 'NONE', ( #1949, #123, #881, #1613, #1745 ) ) ;
#1201 = DIRECTION ( 'NONE',  ( 1.000000000000000000, -5.204170427930417339E-16, 0.000000000000000000 ) ) ;
#1202 = ORIENTED_EDGE ( 'NONE', *, *, #616, .F. ) ;
#1203 = ORIENTED_EDGE ( 'NONE', *, *, #135, .T. ) ;
#1204 = DIRECTION ( 'NONE',  ( -0.000000000000000000, 1.000000000000000000, -0.000000000000000000 ) ) ;
#1205 = CARTESIAN_POINT ( 'NONE',  ( 145.0000000000000284, 3.000000000000000000, -45.00000000000000000 ) ) ;
#1206 = AXIS2_PLACEMENT_3D ( 'NONE', #1699, #852, #1386 ) ;
#1207 = CARTESIAN_POINT ( 'NONE',  ( 0.000000000000000000, -1.178949249685218748, -2.041999999999998039 ) ) ;
#1208 = ADVANCED_FACE ( 'NONE', ( #1198 ), #673, .F. ) ;
#1209 = ORIENTED_EDGE ( 'NONE', *, *, #522, .T. ) ;
#1210 = CIRCLE ( 'NONE', #1149, 2.649999999999985700 ) ;
#1211 = DIRECTION ( 'NONE',  ( 0.000000000000000000, 0.000000000000000000, 1.000000000000000000 ) ) ;
#1212 = DIRECTION ( 'NONE',  ( 0.000000000000000000, 0.4999999999999992784, -0.8660254037844389297 ) ) ;
#1213 = ADVANCED_FACE ( 'NONE', ( #1574 ), #1852, .F. ) ;
#1214 = ADVANCED_FACE ( 'NONE', ( #1233 ), #389, .F. ) ;
#1215 = CARTESIAN_POINT ( 'NONE',  ( -145.0000000000000284, -15.00000000000003197, -42.49999999999999289 ) ) ;
#1216 = VECTOR ( 'NONE', #371, 999.9999999999997726 ) ;
#1217 =( NAMED_UNIT ( * ) SI_UNIT ( $, .STERADIAN. ) SOLID_ANGLE_UNIT ( ) );
#1218 = ORIENTED_EDGE ( 'NONE', *, *, #2178, .T. ) ;
#1219 = DIRECTION ( 'NONE',  ( -0.000000000000000000, 1.000000000000000000, -0.000000000000000000 ) ) ;
#1220 = CARTESIAN_POINT ( 'NONE',  ( -139.9999999999999716, -120.0000000000000142, -40.00000000000000000 ) ) ;
#1221 = FACE_OUTER_BOUND ( 'NONE', #715, .T. ) ;
#1222 = PRODUCT_DEFINITION_FORMATION_WITH_SPECIFIED_SOURCE ( 'ANY', '', #118, .NOT_KNOWN. ) ;
#1223 = AXIS2_PLACEMENT_3D ( 'NONE', #582, #1666, #128 ) ;
#1224 = CIRCLE ( 'NONE', #624, 4.250000000000000000 ) ;
#1225 = VECTOR ( 'NONE', #1671, 1000.000000000000000 ) ;
#1226 = ADVANCED_BREP_SHAPE_REPRESENTATION ( '', ( #1685, #30 ), #1018 ) ;
#1227 = DIRECTION ( 'NONE',  ( 1.000000000000000000, 0.000000000000000000, 0.000000000000000000 ) ) ;
#1228 = CARTESIAN_POINT ( 'NONE',  ( -145.0000000000000284, 2.993649167310367343, -42.35000000000001563 ) ) ;
#1229 = LINE ( 'NONE', #43, #2010 ) ;
#1230 = ORIENTED_EDGE ( 'NONE', *, *, #467, .T. ) ;
#1231 = ORIENTED_EDGE ( 'NONE', *, *, #765, .F. ) ;
#1232 = FACE_OUTER_BOUND ( 'NONE', #2085, .T. ) ;
#1233 = FACE_OUTER_BOUND ( 'NONE', #783, .T. ) ;
#1234 = LINE ( 'NONE', #1918, #1799 ) ;
#1235 = LINE ( 'NONE', #711, #338 ) ;
#1236 = EDGE_CURVE ( 'NONE', #2218, #1159, #635, .T. ) ;
#1237 = AXIS2_PLACEMENT_3D ( 'NONE', #552, #1528, #530 ) ;
#1238 = CARTESIAN_POINT ( 'NONE',  ( 2.500000000000000000, 2.357898499370431722, -2.818925648462311528E-15 ) ) ;
#1239 = ADVANCED_FACE ( 'NONE', ( #179 ), #1564, .T. ) ;
#1240 = CARTESIAN_POINT ( 'NONE',  ( 145.0000000000000284, 2.993649167310367343, 47.64999999999998437 ) ) ;
#1241 = EDGE_CURVE ( 'NONE', #473, #665, #2175, .T. ) ;
#1242 = AXIS2_PLACEMENT_3D ( 'NONE', #25, #862, #419 ) ;
#1243 = ORIENTED_EDGE ( 'NONE', *, *, #2133, .F. ) ;
#1244 = EDGE_LOOP ( 'NONE', ( #465, #2106, #1758, #1172 ) ) ;
#1245 = CYLINDRICAL_SURFACE ( 'NONE', #2102, 2.500000000000002220 ) ;
#1246 = CARTESIAN_POINT ( 'NONE',  ( 0.000000000000000000, 3.000000000000000000, 57.00000000000000711 ) ) ;
#1247 = DIRECTION ( 'NONE',  ( 0.000000000000000000, 0.000000000000000000, -1.000000000000000000 ) ) ;
#1248 = ORIENTED_EDGE ( 'NONE', *, *, #1383, .F. ) ;
#1249 = CARTESIAN_POINT ( 'NONE',  ( 145.0000000000000284, 0.000000000000000000, -47.64999999999998437 ) ) ;
#1250 = AXIS2_PLACEMENT_3D ( 'NONE', #439, #1118, #1801 ) ;
#1251 = DIRECTION ( 'NONE',  ( 2.312964634635742957E-16, 0.000000000000000000, -1.000000000000000000 ) ) ;
#1252 = AXIS2_PLACEMENT_3D ( 'NONE', #149, #1020, #1319 ) ;
#1253 = VECTOR ( 'NONE', #1084, 1000.000000000000000 ) ;
#1254 = ORIENTED_EDGE ( 'NONE', *, *, #518, .F. ) ;
#1255 = VERTEX_POINT ( 'NONE', #1040 ) ;
#1256 = FACE_OUTER_BOUND ( 'NONE', #1318, .T. ) ;
#1257 = LINE ( 'NONE', #47, #418 ) ;
#1258 = CARTESIAN_POINT ( 'NONE',  ( 5.200000000000002842, 3.306546357697854226E-16, 2.700000000000000622 ) ) ;
#1259 = ADVANCED_FACE ( 'NONE', ( #690 ), #1556, .T. ) ;
#1260 = CARTESIAN_POINT ( 'NONE',  ( 21.00000000000000355, 0.000000000000000000, 2.055000000000000160 ) ) ;
#1261 = VECTOR ( 'NONE', #1655, 1000.000000000000114 ) ;
#1262 = AXIS2_PLACEMENT_3D ( 'NONE', #846, #867, #2031 ) ;
#1263 = FACE_OUTER_BOUND ( 'NONE', #349, .T. ) ;
#1264 = AXIS2_PLACEMENT_3D ( 'NONE', #1273, #1954, #1296 ) ;
#1265 = FILL_AREA_STYLE_COLOUR ( '', #361 ) ;
#1266 = EDGE_LOOP ( 'NONE', ( #994, #322, #1098, #688, #1580 ) ) ;
#1267 = ADVANCED_FACE ( 'NONE', ( #1368 ), #8, .T. ) ;
#1268 = EDGE_LOOP ( 'NONE', ( #407, #911, #1644, #294 ) ) ;
#1269 = CARTESIAN_POINT ( 'NONE',  ( -145.0000000000000284, 2.800000000000000266, -45.00000000000000000 ) ) ;
#1270 = DIRECTION ( 'NONE',  ( 0.000000000000000000, 0.000000000000000000, -1.000000000000000000 ) ) ;
#1271 = CARTESIAN_POINT ( 'NONE',  ( 0.000000000000000000, -1.178949249685214307, 2.042000000000001592 ) ) ;
#1272 = EDGE_CURVE ( 'NONE', #665, #1159, #2137, .T. ) ;
#1273 = CARTESIAN_POINT ( 'NONE',  ( 20.55500000000001748, 0.000000000000000000, 0.000000000000000000 ) ) ;
#1274 = CYLINDRICAL_SURFACE ( 'NONE', #2189, 4.250000000000000000 ) ;
#1275 = CARTESIAN_POINT ( 'NONE',  ( 145.0000000000000284, 0.000000000000000000, 42.35000000000001563 ) ) ;
#1276 = AXIS2_PLACEMENT_3D ( 'NONE', #1346, #2162, #289 ) ;
#1277 = ORIENTED_EDGE ( 'NONE', *, *, #186, .F. ) ;
#1278 = ORIENTED_EDGE ( 'NONE', *, *, #1197, .T. ) ;
#1279 = AXIS2_PLACEMENT_3D ( 'NONE', #2108, #1940, #408 ) ;
#1280 = DIRECTION ( 'NONE',  ( 0.000000000000000000, 0.000000000000000000, 1.000000000000000000 ) ) ;
#1281 = CARTESIAN_POINT ( 'NONE',  ( 0.000000000000000000, 0.000000000000000000, -50.00000000000000000 ) ) ;
#1282 = PRODUCT_DEFINITION_SHAPE ( 'NONE', 'NONE',  #2230 ) ;
#1284 = VERTEX_POINT ( 'NONE', #1563 ) ;
#1283 = CARTESIAN_POINT ( 'NONE',  ( 21.00000000000000000, 2.055000000000000160, 0.000000000000000000 ) ) ;
#1285 = CIRCLE ( 'NONE', #1105, 4.250000000000000000 ) ;
#1286 = PLANE ( 'NONE',  #714 ) ;
#1287 = DIRECTION ( 'NONE',  ( 0.000000000000000000, -0.000000000000000000, -1.000000000000000000 ) ) ;
#1288 = APPLICATION_PROTOCOL_DEFINITION ( 'draft international standard', 'automotive_design', 1998, #1501 ) ;
#1289 = ORIENTED_EDGE ( 'NONE', *, *, #416, .F. ) ;
#1290 = ORIENTED_EDGE ( 'NONE', *, *, #1143, .F. ) ;
#1291 = DIRECTION ( 'NONE',  ( 6.123233995736766036E-17, -1.000000000000000000, 0.000000000000000000 ) ) ;
#1292 = CARTESIAN_POINT ( 'NONE',  ( 2.500000000000000000, -2.629050547790028551E-15, -2.041999999999999815 ) ) ;
#1293 = VERTEX_POINT ( 'NONE', #366 ) ;
#1295 = ORIENTED_EDGE ( 'NONE', *, *, #880, .F. ) ;
#1294 = CARTESIAN_POINT ( 'NONE',  ( -139.9999999999999716, -120.0000000000000142, -50.00000000000000000 ) ) ;
#1296 = DIRECTION ( 'NONE',  ( 0.000000000000000000, 0.000000000000000000, 1.000000000000000000 ) ) ;
#1297 = FACE_BOUND ( 'NONE', #2001, .T. ) ;
#1298 = FACE_OUTER_BOUND ( 'NONE', #1677, .T. ) ;
#1299 = ADVANCED_FACE ( 'NONE', ( #708 ), #1031, .T. ) ;
#1300 = VECTOR ( 'NONE', #1720, 1000.000000000000000 ) ;
#1301 = CONICAL_SURFACE ( 'NONE', #1122, 2.500000000000002220, 1.029744258676654534 ) ;
#1302 = EDGE_LOOP ( 'NONE', ( #2097, #1843, #947, #280 ) ) ;
#1303 = ORIENTED_EDGE ( 'NONE', *, *, #698, .F. ) ;
#1304 = CIRCLE ( 'NONE', #177, 2.649999999999985700 ) ;
#1305 = CARTESIAN_POINT ( 'NONE',  ( -145.0000000000000284, 3.000000000000001776, -42.29999999999999716 ) ) ;
#1306 = ORIENTED_EDGE ( 'NONE', *, *, #1923, .F. ) ;
#1307 = DIRECTION ( 'NONE',  ( 0.000000000000000000, 0.000000000000000000, -1.000000000000000000 ) ) ;
#1308 = CARTESIAN_POINT ( 'NONE',  ( 2.500000000000000000, 2.357898499370431722, -2.818925648462311528E-15 ) ) ;
#1309 = EDGE_CURVE ( 'NONE', #1470, #226, #856, .T. ) ;
#1310 = CARTESIAN_POINT ( 'NONE',  ( 145.0000000000000284, 3.000000000000000000, 47.64999999999998437 ) ) ;
#1311 =( LENGTH_UNIT ( ) NAMED_UNIT ( * ) SI_UNIT ( .MILLI., .METRE. ) );
#1312 = EDGE_CURVE ( 'NONE', #2144, #2205, #1965, .T. ) ;
#1313 = DIRECTION ( 'NONE',  ( 0.000000000000000000, 0.000000000000000000, 1.000000000000000000 ) ) ;
#1314 = EDGE_CURVE ( 'NONE', #1439, #353, #1257, .T. ) ;
#1315 = EDGE_CURVE ( 'NONE', #1663, #1188, #997, .T. ) ;
#1316 = VERTEX_POINT ( 'NONE', #1582 ) ;
#1317 = DIRECTION ( 'NONE',  ( -2.312964634635742957E-16, 0.000000000000000000, 1.000000000000000000 ) ) ;
#1318 = EDGE_LOOP ( 'NONE', ( #100, #695, #2130, #251 ) ) ;
#1319 = DIRECTION ( 'NONE',  ( 0.000000000000000000, 0.000000000000000000, 1.000000000000000000 ) ) ;
#1320 = CARTESIAN_POINT ( 'NONE',  ( -145.0000000000000284, 3.000000000000002665, -45.00000000000000000 ) ) ;
#1321 = AXIS2_PLACEMENT_3D ( 'NONE', #1283, #382, #1307 ) ;
#1322 = DIRECTION ( 'NONE',  ( 0.000000000000000000, 0.000000000000000000, -1.000000000000000000 ) ) ;
#1323 = DIRECTION ( 'NONE',  ( 6.123233995736766036E-17, -1.000000000000000000, 0.000000000000000000 ) ) ;
#1324 = MECHANICAL_DESIGN_GEOMETRIC_PRESENTATION_REPRESENTATION (  '', ( #1329 ), #932 ) ;
#1325 = ITEM_DEFINED_TRANSFORMATION ( 'NONE', 'NONE', #691,  #30 ) ;
#1326 = ORIENTED_EDGE ( 'NONE', *, *, #931, .T. ) ;
#1327 = DIRECTION ( 'NONE',  ( 0.000000000000000000, -1.000000000000000000, 0.000000000000000000 ) ) ;
#1328 = ORIENTED_EDGE ( 'NONE', *, *, #910, .T. ) ;
#1329=STYLED_ITEM('',(#2254),#1673);
#1330 = FACE_OUTER_BOUND ( 'NONE', #1451, .T. ) ;
#1331 = EDGE_CURVE ( 'NONE', #1125, #705, #12, .T. ) ;
#1332 = CARTESIAN_POINT ( 'NONE',  ( -149.9999999999999716, -120.0000000000000142, -40.00000000000000000 ) ) ;
#1333 = EDGE_CURVE ( 'NONE', #1509, #1909, #1078, .T. ) ;
#1334 = ORIENTED_EDGE ( 'NONE', *, *, #567, .T. ) ;
#1335 = PLANE ( 'NONE',  #1585 ) ;
#1336 = CARTESIAN_POINT ( 'NONE',  ( -139.9999999999999716, 2.312964634635743056E-15, 50.00000000000000000 ) ) ;
#1337 = DIRECTION ( 'NONE',  ( 1.000000000000000000, 0.000000000000000000, 0.000000000000000000 ) ) ;
#1338 = AXIS2_PLACEMENT_3D ( 'NONE', #1108, #1313, #278 ) ;
#1339 = CIRCLE ( 'NONE', #1406, 2.500000000000002220 ) ;
#1340 = CIRCLE ( 'NONE', #1021, 2.700000000000000622 ) ;
#1341 = ORIENTED_EDGE ( 'NONE', *, *, #2196, .F. ) ;
#1342 = DIRECTION ( 'NONE',  ( 0.000000000000000000, 0.000000000000000000, 1.000000000000000000 ) ) ;
#1343 = ORIENTED_EDGE ( 'NONE', *, *, #232, .F. ) ;
#1344 = EDGE_CURVE ( 'NONE', #1831, #1569, #948, .T. ) ;
#1345 = DIRECTION ( 'NONE',  ( 0.000000000000000000, 0.000000000000000000, 1.000000000000000000 ) ) ;
#1346 = CARTESIAN_POINT ( 'NONE',  ( -145.0000000000000284, -3.358697307418414604E-14, 45.00000000000000000 ) ) ;
#1347 = ADVANCED_FACE ( 'NONE', ( #1433, #1089 ), #1614, .T. ) ;
#1348 = VERTEX_POINT ( 'NONE', #58 ) ;
#1349 = CARTESIAN_POINT ( 'NONE',  ( 159.9999999999999716, 10.00000000000000000, 60.00000000000001421 ) ) ;
#1350 = DIRECTION ( 'NONE',  ( 1.000000000000000000, 2.312964634635742957E-16, -0.000000000000000000 ) ) ;
#1351 = DIRECTION ( 'NONE',  ( 0.000000000000000000, 0.000000000000000000, 1.000000000000000000 ) ) ;
#1352 = ORIENTED_EDGE ( 'NONE', *, *, #1697, .F. ) ;
#1353 = VERTEX_POINT ( 'NONE', #562 ) ;
#1354 = AXIS2_PLACEMENT_3D ( 'NONE', #718, #1718, #2076 ) ;
#1355 = CARTESIAN_POINT ( 'NONE',  ( 0.000000000000000000, 2.357898499370431722, -2.818925648462311528E-15 ) ) ;
#1356 = DIRECTION ( 'NONE',  ( -0.000000000000000000, 1.000000000000000000, -0.000000000000000000 ) ) ;
#1357 = UNCERTAINTY_MEASURE_WITH_UNIT (LENGTH_MEASURE( 1.000000000000000082E-05 ), #618, 'distance_accuracy_value', 'NONE');
#1358 = VERTEX_POINT ( 'NONE', #1416 ) ;
#1359 = DIRECTION ( 'NONE',  ( -0.000000000000000000, 1.000000000000000000, -0.000000000000000000 ) ) ;
#1360 = CIRCLE ( 'NONE', #1420, 0.2500000000000002220 ) ;
#1361 = LINE ( 'NONE', #1575, #429 ) ;
#1362 = FILL_AREA_STYLE ('',( #2225 ) ) ;
#1363 = EDGE_CURVE ( 'NONE', #405, #2192, #233, .T. ) ;
#1364 = EDGE_LOOP ( 'NONE', ( #442, #915, #824, #454, #452 ) ) ;
#1365 = AXIS2_PLACEMENT_3D ( 'NONE', #1732, #1812, #1154 ) ;
#1366 = ORIENTED_EDGE ( 'NONE', *, *, #2105, .T. ) ;
#1367 = DIRECTION ( 'NONE',  ( -1.000000000000000000, -6.123233995736766036E-17, -0.000000000000000000 ) ) ;
#1368 = FACE_OUTER_BOUND ( 'NONE', #140, .T. ) ;
#1369 = VECTOR ( 'NONE', #851, 1000.000000000000000 ) ;
#1370 = VECTOR ( 'NONE', #243, 1000.000000000000000 ) ;
#1371 = ORIENTED_EDGE ( 'NONE', *, *, #645, .T. ) ;
#1372 = LINE ( 'NONE', #1058, #1692 ) ;
#1373 = ADVANCED_FACE ( 'NONE', ( #753 ), #1425, .F. ) ;
#1374 = ORIENTED_EDGE ( 'NONE', *, *, #1767, .F. ) ;
#1375 = ORIENTED_EDGE ( 'NONE', *, *, #1363, .T. ) ;
#1376 = CIRCLE ( 'NONE', #406, 2.041999999999999815 ) ;
#1377 = CARTESIAN_POINT ( 'NONE',  ( 145.0000000000000284, 0.000000000000000000, 47.64999999999998437 ) ) ;
#1378 = DIRECTION ( 'NONE',  ( 0.000000000000000000, 0.000000000000000000, 1.000000000000000000 ) ) ;
#1379 = CARTESIAN_POINT ( 'NONE',  ( -157.0000000000000284, 10.00000000000000000, 57.00000000000000711 ) ) ;
#1380 = ADVANCED_FACE ( 'NONE', ( #400 ), #1112, .F. ) ;
#1381 =( LENGTH_UNIT ( ) NAMED_UNIT ( * ) SI_UNIT ( .MILLI., .METRE. ) );
#1382 = EDGE_LOOP ( 'NONE', ( #1870, #332, #1278, #780 ) ) ;
#1383 = EDGE_CURVE ( 'NONE', #1725, #898, #1210, .T. ) ;
#1384 = ORIENTED_EDGE ( 'NONE', *, *, #746, .T. ) ;
#1385 = FACE_OUTER_BOUND ( 'NONE', #1859, .T. ) ;
#1386 = DIRECTION ( 'NONE',  ( 0.000000000000000000, 0.000000000000000000, 1.000000000000000000 ) ) ;
#1387 = CIRCLE ( 'NONE', #1886, 2.500000000000002220 ) ;
#1388 = DIRECTION ( 'NONE',  ( 0.000000000000000000, 0.000000000000000000, -1.000000000000000000 ) ) ;
#1389 =( NAMED_UNIT ( * ) PLANE_ANGLE_UNIT ( ) SI_UNIT ( $, .RADIAN. ) );
#1390 = VERTEX_POINT ( 'NONE', #1792 ) ;
#1391 = AXIS2_PLACEMENT_3D ( 'NONE', #1336, #832, #340 ) ;
#1392 = CARTESIAN_POINT ( 'NONE',  ( 145.0000000000000284, 3.000000000000000000, 45.00000000000000000 ) ) ;
#1393 = CARTESIAN_POINT ( 'NONE',  ( -160.0000000000000284, 10.00000000000000000, 57.00000000000000711 ) ) ;
#1394 = CARTESIAN_POINT ( 'NONE',  ( 145.0000000000000284, 2.800000000000000266, 47.70000000000000284 ) ) ;
#1395 = EDGE_CURVE ( 'NONE', #353, #256, #934, .T. ) ;
#1396 = ORIENTED_EDGE ( 'NONE', *, *, #1383, .T. ) ;
#1397 = ADVANCED_FACE ( 'NONE', ( #82 ), #595, .F. ) ;
#1398 = CONICAL_SURFACE ( 'NONE', #1719, 2.055000000000000160, 0.7853981633974639331 ) ;
#1399 = PLANE ( 'NONE',  #1435 ) ;
#1400 = SURFACE_STYLE_USAGE ( .BOTH. , #1567 ) ;
#1401 = ORIENTED_EDGE ( 'NONE', *, *, #541, .F. ) ;
#1402 = ORIENTED_EDGE ( 'NONE', *, *, #1103, .F. ) ;
#1403 = CARTESIAN_POINT ( 'NONE',  ( -145.0000000000000284, 2.993649167310367343, 47.64999999999998437 ) ) ;
#1404 = CARTESIAN_POINT ( 'NONE',  ( 2.500000000000000000, -1.768423874527823569, 1.021000000000002350 ) ) ;
#1405 = CARTESIAN_POINT ( 'NONE',  ( -145.0000000000000284, 3.000000000000000000, 45.00000000000000000 ) ) ;
#1406 = AXIS2_PLACEMENT_3D ( 'NONE', #1153, #1359, #2185 ) ;
#1407 = AXIS2_PLACEMENT_3D ( 'NONE', #200, #692, #720 ) ;
#1408 = AXIS2_PLACEMENT_3D ( 'NONE', #609, #1966, #1079 ) ;
#1409 = CARTESIAN_POINT ( 'NONE',  ( -139.9999999999999716, 2.312964634635743056E-15, 50.00000000000000000 ) ) ;
#1410 = PRODUCT_DEFINITION ( 'UNKNOWN', '', #836, #2052 ) ;
#1411 = CARTESIAN_POINT ( 'NONE',  ( -145.0000000000000284, -15.00000000000003197, -45.00000000000000000 ) ) ;
#1412 = CARTESIAN_POINT ( 'NONE',  ( 0.2500000000000002220, 0.000000000000000000, 4.250000000000000000 ) ) ;
#1413 = ORIENTED_EDGE ( 'NONE', *, *, #1181, .F. ) ;
#1414 = ORIENTED_EDGE ( 'NONE', *, *, #10, .T. ) ;
#1415 = CARTESIAN_POINT ( 'NONE',  ( 145.0000000000000284, 0.000000000000000000, 45.00000000000000000 ) ) ;
#1416 = CARTESIAN_POINT ( 'NONE',  ( 21.00000000000000355, 0.000000000000000000, 2.055000000000000160 ) ) ;
#1417 = FACE_OUTER_BOUND ( 'NONE', #1266, .T. ) ;
#1418 = CARTESIAN_POINT ( 'NONE',  ( 0.000000000000000000, 1.178949249685217415, 2.041999999999998483 ) ) ;
#1419 = FILL_AREA_STYLE ('',( #1922 ) ) ;
#1420 = AXIS2_PLACEMENT_3D ( 'NONE', #1099, #1780, #1088 ) ;
#1421 = VERTEX_POINT ( 'NONE', #1627 ) ;
#1422 = EDGE_CURVE ( 'NONE', #694, #1700, #2145, .T. ) ;
#1423 = EDGE_LOOP ( 'NONE', ( #619, #1895, #1589, #631 ) ) ;
#1424 = CARTESIAN_POINT ( 'NONE',  ( -145.0000000000000284, 3.000000000000002665, 45.00000000000000000 ) ) ;
#1425 = PLANE ( 'NONE',  #685 ) ;
#1426 = CARTESIAN_POINT ( 'NONE',  ( -160.0000000000000000, 10.00000000000000000, -59.99999999999998579 ) ) ;
#1427 = DIRECTION ( 'NONE',  ( 0.000000000000000000, -0.000000000000000000, -1.000000000000000000 ) ) ;
#1428 = SURFACE_STYLE_FILL_AREA ( #1419 ) ;
#1429 = CIRCLE ( 'NONE', #1148, 2.055000000000000160 ) ;
#1430 = VERTEX_POINT ( 'NONE', #1760 ) ;
#1431 = EDGE_LOOP ( 'NONE', ( #328, #1162, #1193 ) ) ;
#1432 = LINE ( 'NONE', #1071, #1817 ) ;
#1433 = FACE_BOUND ( 'NONE', #871, .T. ) ;
#1434 = CARTESIAN_POINT ( 'NONE',  ( 0.000000000000000000, 3.000000000000000000, 0.000000000000000000 ) ) ;
#1435 = AXIS2_PLACEMENT_3D ( 'NONE', #239, #85, #961 ) ;
#1436 = AXIS2_PLACEMENT_3D ( 'NONE', #1281, #1068, #421 ) ;
#1437 = CARTESIAN_POINT ( 'NONE',  ( 0.000000000000000000, 2.357898499370431722, -2.818925648462311528E-15 ) ) ;
#1438 = ORIENTED_EDGE ( 'NONE', *, *, #1751, .T. ) ;
#1439 = VERTEX_POINT ( 'NONE', #218 ) ;
#1440 = ADVANCED_FACE ( 'NONE', ( #1806 ), #958, .F. ) ;
#1441 = DIRECTION ( 'NONE',  ( -0.000000000000000000, 1.000000000000000000, -0.000000000000000000 ) ) ;
#1442 = DIRECTION ( 'NONE',  ( 0.000000000000000000, 0.000000000000000000, -1.000000000000000000 ) ) ;
#1444 = VERTEX_POINT ( 'NONE', #443 ) ;
#1443 = DIRECTION ( 'NONE',  ( -1.000000000000000000, 0.000000000000000000, 0.000000000000000000 ) ) ;
#1445 =( NAMED_UNIT ( * ) SI_UNIT ( $, .STERADIAN. ) SOLID_ANGLE_UNIT ( ) );
#1446 = CARTESIAN_POINT ( 'NONE',  ( -145.0000000000000284, -15.00000000000003197, 45.00000000000000000 ) ) ;
#1447 = CARTESIAN_POINT ( 'NONE',  ( 0.000000000000000000, 10.00000000000000000, 57.00000000000000711 ) ) ;
#1448 = VECTOR ( 'NONE', #1152, 1000.000000000000000 ) ;
#1449 = PRODUCT_CONTEXT ( 'NONE', #849, 'mechanical' ) ;
#1450 = SURFACE_SIDE_STYLE ('',( #1499 ) ) ;
#1451 = EDGE_LOOP ( 'NONE', ( #1127, #560, #24, #1192 ) ) ;
#1452 = ORIENTED_EDGE ( 'NONE', *, *, #384, .T. ) ;
#1453 = VECTOR ( 'NONE', #435, 1000.000000000000114 ) ;
#1454 = CARTESIAN_POINT ( 'NONE',  ( 145.0000000000000284, 0.000000000000000000, -45.00000000000000000 ) ) ;
#1455 = LINE ( 'NONE', #1271, #480 ) ;
#1456 = ORIENTED_EDGE ( 'NONE', *, *, #55, .F. ) ;
#1458 = ORIENTED_EDGE ( 'NONE', *, *, #121, .F. ) ;
#1457 = DIRECTION ( 'NONE',  ( 0.000000000000000000, 0.000000000000000000, 1.000000000000000000 ) ) ;
#1459 = DIRECTION ( 'NONE',  ( 0.000000000000000000, -1.000000000000000000, 0.000000000000000000 ) ) ;
#1460 = AXIS2_PLACEMENT_3D ( 'NONE', #317, #377, #142 ) ;
#1461 = CARTESIAN_POINT ( 'NONE',  ( -145.0000000000000284, 0.000000000000000000, -47.64999999999998437 ) ) ;
#1462 = CONTEXT_DEPENDENT_SHAPE_REPRESENTATION ( #1045, #257 ) ;
#1463 = AXIS2_PLACEMENT_3D ( 'NONE', #2038, #658, #1151 ) ;
#1464 = AXIS2_PLACEMENT_3D ( 'NONE', #1781, #252, #1280 ) ;
#1465 = VERTEX_POINT ( 'NONE', #2139 ) ;
#1466 = ORIENTED_EDGE ( 'NONE', *, *, #1075, .F. ) ;
#1467 = DIRECTION ( 'NONE',  ( -0.7071067811865364705, 8.659560562355067211E-17, -0.7071067811865584529 ) ) ;
#1468 = ORIENTED_EDGE ( 'NONE', *, *, #1588, .F. ) ;
#1470 = VERTEX_POINT ( 'NONE', #602 ) ;
#1469 = LINE ( 'NONE', #1911, #152 ) ;
#1471 = CARTESIAN_POINT ( 'NONE',  ( -145.0000000000000284, -15.00000000000003197, 42.49999999999999289 ) ) ;
#1472 = ADVANCED_FACE ( 'NONE', ( #426, #590, #1297, #1800, #1117 ), #1286, .T. ) ;
#1473 = EDGE_CURVE ( 'NONE', #898, #216, #745, .T. ) ;
#1474 = LINE ( 'NONE', #1310, #1605 ) ;
#1475 = CARTESIAN_POINT ( 'NONE',  ( -150.0000000000000000, 0.000000000000000000, 50.00000000000000000 ) ) ;
#1476 =( GEOMETRIC_REPRESENTATION_CONTEXT ( 3 ) GLOBAL_UNCERTAINTY_ASSIGNED_CONTEXT ( ( #1711 ) ) GLOBAL_UNIT_ASSIGNED_CONTEXT ( ( #428, #1827, #1478 ) ) REPRESENTATION_CONTEXT ( 'NONE', 'WORKASPACE' ) );
#1477 = APPLICATION_PROTOCOL_DEFINITION ( 'draft international standard', 'automotive_design', 1998, #964 ) ;
#1478 =( NAMED_UNIT ( * ) SI_UNIT ( $, .STERADIAN. ) SOLID_ANGLE_UNIT ( ) );
#1479 = EDGE_LOOP ( 'NONE', ( #108, #1803, #483, #265 ) ) ;
#1480 = LINE ( 'NONE', #2206, #1225 ) ;
#1481 = EDGE_LOOP ( 'NONE', ( #1102, #364, #133, #1008 ) ) ;
#1482 = CARTESIAN_POINT ( 'NONE',  ( 0.000000000000000000, 10.00000000000000000, 0.000000000000000000 ) ) ;
#1483 = DIRECTION ( 'NONE',  ( 0.000000000000000000, 0.000000000000000000, -1.000000000000000000 ) ) ;
#1484 = DIRECTION ( 'NONE',  ( 0.000000000000000000, 1.000000000000000000, -1.287488025362403787E-15 ) ) ;
#1485 = CARTESIAN_POINT ( 'NONE',  ( 157.0000000000000000, 10.00000000000000000, -56.99999999999999289 ) ) ;
#1486 = CONTEXT_DEPENDENT_SHAPE_REPRESENTATION ( #737, #601 ) ;
#1487 =( NAMED_UNIT ( * ) PLANE_ANGLE_UNIT ( ) SI_UNIT ( $, .RADIAN. ) );
#1488 = AXIS2_PLACEMENT_3D ( 'NONE', #513, #1897, #1882 ) ;
#1489 = ADVANCED_FACE ( 'NONE', ( #2114 ), #644, .F. ) ;
#1490 = ORIENTED_EDGE ( 'NONE', *, *, #2067, .T. ) ;
#1491 = LINE ( 'NONE', #284, #1620 ) ;
#1492 = EDGE_CURVE ( 'NONE', #1531, #344, #1304, .T. ) ;
#1493 = ORIENTED_EDGE ( 'NONE', *, *, #1772, .F. ) ;
#1494 = LINE ( 'NONE', #1653, #1930 ) ;
#1495 = DIRECTION ( 'NONE',  ( -6.123233995736766036E-17, 1.000000000000000000, -0.000000000000000000 ) ) ;
#1496 = CARTESIAN_POINT ( 'NONE',  ( 145.0000000000000284, 0.000000000000000000, -45.00000000000000000 ) ) ;
#1497 = DIRECTION ( 'NONE',  ( 0.000000000000000000, 0.000000000000000000, -1.000000000000000000 ) ) ;
#1498 = CONICAL_SURFACE ( 'NONE', #533, 2.500000000000002220, 1.029744258676654534 ) ;
#1499 = SURFACE_STYLE_FILL_AREA ( #2154 ) ;
#1500 = ADVANCED_FACE ( 'NONE', ( #1263 ), #1274, .T. ) ;
#1501 = APPLICATION_CONTEXT ( 'automotive_design' ) ;
#1502 = ORIENTED_EDGE ( 'NONE', *, *, #1893, .T. ) ;
#1503 = ADVANCED_FACE ( 'NONE', ( #786 ), #771, .F. ) ;
#1504 = DIRECTION ( 'NONE',  ( 0.000000000000000000, 0.000000000000000000, 1.000000000000000000 ) ) ;
#1505 = VERTEX_POINT ( 'NONE', #1437 ) ;
#1506=STYLED_ITEM('',(#2268),#1685);
#1507 = LINE ( 'NONE', #1355, #1063 ) ;
#1508 = LINE ( 'NONE', #335, #1448 ) ;
#1509 = VERTEX_POINT ( 'NONE', #1947 ) ;
#1510 = CARTESIAN_POINT ( 'NONE',  ( -160.0000000000000000, 10.00000000000000000, -59.99999999999998579 ) ) ;
#1511 = CARTESIAN_POINT ( 'NONE',  ( 2.500000000000000000, 0.000000000000000000, 0.000000000000000000 ) ) ;
#1512 = ORIENTED_EDGE ( 'NONE', *, *, #121, .T. ) ;
#1513 = CIRCLE ( 'NONE', #579, 2.500000000000002220 ) ;
#1514 = TOROIDAL_SURFACE ( 'NONE', #1083, 2.700000000000000622, 0.2000000000000000111 ) ;
#1515 = ORIENTED_EDGE ( 'NONE', *, *, #477, .T. ) ;
#1516 = LINE ( 'NONE', #269, #372 ) ;
#1517 = ORIENTED_EDGE ( 'NONE', *, *, #1850, .T. ) ;
#1518 = PLANE ( 'NONE',  #569 ) ;
#1519 = DIRECTION ( 'NONE',  ( 1.000000000000000000, 0.000000000000000000, 0.000000000000000000 ) ) ;
#1520 = ORIENTED_EDGE ( 'NONE', *, *, #13, .T. ) ;
#1521 = LINE ( 'NONE', #1349, #250 ) ;
#1522 = CARTESIAN_POINT ( 'NONE',  ( 2.500000000000000000, 2.357898499370431722, -2.818925648462311528E-15 ) ) ;
#1523 = CARTESIAN_POINT ( 'NONE',  ( 145.0000000000000284, 8.000000000000003553, 45.00000000000000000 ) ) ;
#1524 = ORIENTED_EDGE ( 'NONE', *, *, #706, .F. ) ;
#1525 = EDGE_LOOP ( 'NONE', ( #710, #1846, #445, #766, #1243, #1652, #550, #56 ) ) ;
#1526 = AXIS2_PLACEMENT_3D ( 'NONE', #2183, #326, #1519 ) ;
#1527 = FACE_OUTER_BOUND ( 'NONE', #32, .T. ) ;
#1528 = DIRECTION ( 'NONE',  ( 6.123233995736766036E-17, -1.000000000000000000, 0.000000000000000000 ) ) ;
#1529 = UNCERTAINTY_MEASURE_WITH_UNIT (LENGTH_MEASURE( 1.000000000000000082E-05 ), #1311, 'distance_accuracy_value', 'NONE');
#1530 = ADVANCED_FACE ( 'NONE', ( #1622 ), #1498, .F. ) ;
#1531 = VERTEX_POINT ( 'NONE', #1461 ) ;
#1532 = LINE ( 'NONE', #1848, #1875 ) ;
#1533 = CIRCLE ( 'NONE', #2037, 2.500000000000000444 ) ;
#1534 = DIRECTION ( 'NONE',  ( 0.000000000000000000, 0.000000000000000000, -1.000000000000000000 ) ) ;
#1535 =( LENGTH_UNIT ( ) NAMED_UNIT ( * ) SI_UNIT ( .MILLI., .METRE. ) );
#1536 = ORIENTED_EDGE ( 'NONE', *, *, #748, .T. ) ;
#1537 = EDGE_LOOP ( 'NONE', ( #1810, #1202, #729, #558, #1384 ) ) ;
#1538 = DIRECTION ( 'NONE',  ( -0.000000000000000000, 1.000000000000000000, -0.000000000000000000 ) ) ;
#1539 = CARTESIAN_POINT ( 'NONE',  ( 2.500000000000000000, 0.000000000000000000, 0.000000000000000000 ) ) ;
#1540 = AXIS2_PLACEMENT_3D ( 'NONE', #1482, #159, #1844 ) ;
#1541 = VECTOR ( 'NONE', #1067, 1000.000000000000000 ) ;
#1542 = EDGE_CURVE ( 'NONE', #899, #94, #1754, .T. ) ;
#1543 = ORIENTED_EDGE ( 'NONE', *, *, #1850, .F. ) ;
#1544 = EDGE_CURVE ( 'NONE', #835, #1255, #1106, .T. ) ;
#1545 = CARTESIAN_POINT ( 'NONE',  ( -160.0000000000000000, 10.00000000000000000, -59.99999999999998579 ) ) ;
#1546 = ADVANCED_FACE ( 'NONE', ( #757 ), #1398, .T. ) ;
#1547 = EDGE_CURVE ( 'NONE', #44, #653, #577, .T. ) ;
#1548 = SURFACE_STYLE_USAGE ( .BOTH. , #143 ) ;
#1549 = STYLED_ITEM ( 'NONE', ( #319 ), #1226 ) ;
#1550 = ORIENTED_EDGE ( 'NONE', *, *, #1568, .F. ) ;
#1551 = VECTOR ( 'NONE', #201, 1000.000000000000000 ) ;
#1552 = ORIENTED_EDGE ( 'NONE', *, *, #993, .F. ) ;
#1553 = VECTOR ( 'NONE', #134, 1000.000000000000000 ) ;
#1554 = AXIS2_PLACEMENT_3D ( 'NONE', #448, #50, #2136 ) ;
#1555 = CARTESIAN_POINT ( 'NONE',  ( -160.0000000000000000, 0.000000000000000000, -59.99999999999998579 ) ) ;
#1556 = PLANE ( 'NONE',  #274 ) ;
#1557 = CARTESIAN_POINT ( 'NONE',  ( -150.0000000000000000, 0.000000000000000000, -50.00000000000000000 ) ) ;
#1558 =( NAMED_UNIT ( * ) PLANE_ANGLE_UNIT ( ) SI_UNIT ( $, .RADIAN. ) );
#1559 = ORIENTED_EDGE ( 'NONE', *, *, #1568, .T. ) ;
#1560 = ADVANCED_FACE ( 'NONE', ( #968, #1647 ), #938, .T. ) ;
#1561 = DIRECTION ( 'NONE',  ( -1.000000000000000000, -0.000000000000000000, -0.000000000000000000 ) ) ;
#1562 = ADVANCED_FACE ( 'NONE', ( #1811 ), #750, .F. ) ;
#1563 = CARTESIAN_POINT ( 'NONE',  ( -140.0000000000000000, -10.00000000000000000, -40.00000000000000000 ) ) ;
#1564 = TOROIDAL_SURFACE ( 'NONE', #129, 2.700000000000000622, 0.2000000000000000111 ) ;
#1565 = CARTESIAN_POINT ( 'NONE',  ( 145.0000000000000284, 3.000000000000000000, -42.35000000000001563 ) ) ;
#1566 = CARTESIAN_POINT ( 'NONE',  ( 2.500000000000000000, 0.000000000000000000, 2.041999999999999815 ) ) ;
#1567 = SURFACE_SIDE_STYLE ('',( #1428 ) ) ;
#1568 = EDGE_CURVE ( 'NONE', #240, #1663, #1474, .T. ) ;
#1569 = VERTEX_POINT ( 'NONE', #556 ) ;
#1570 = VECTOR ( 'NONE', #1002, 1000.000000000000000 ) ;
#1571 = EDGE_CURVE ( 'NONE', #805, #324, #1229, .T. ) ;
#1572 = LINE ( 'NONE', #196, #926 ) ;
#1573 = EDGE_CURVE ( 'NONE', #2156, #1883, #1072, .T. ) ;
#1574 = FACE_OUTER_BOUND ( 'NONE', #1964, .T. ) ;
#1575 = CARTESIAN_POINT ( 'NONE',  ( -160.0000000000000284, 0.000000000000000000, 60.00000000000001421 ) ) ;
#1576 = LINE ( 'NONE', #2063, #837 ) ;
#1577 = LINE ( 'NONE', #2149, #906 ) ;
#1578 = DIRECTION ( 'NONE',  ( -0.000000000000000000, -0.000000000000000000, -1.000000000000000000 ) ) ;
#1579 = VERTEX_POINT ( 'NONE', #1412 ) ;
#1580 = ORIENTED_EDGE ( 'NONE', *, *, #40, .T. ) ;
#1581 = DIRECTION ( 'NONE',  ( 0.000000000000000000, 0.000000000000000000, -1.000000000000000000 ) ) ;
#1582 = CARTESIAN_POINT ( 'NONE',  ( 145.0000000000000284, 3.000000000000001776, -42.29999999999999716 ) ) ;
#1583 = DIRECTION ( 'NONE',  ( 0.000000000000000000, 1.224646799147353207E-16, 1.000000000000000000 ) ) ;
#1584 = VECTOR ( 'NONE', #295, 1000.000000000000114 ) ;
#1585 = AXIS2_PLACEMENT_3D ( 'NONE', #844, #1001, #820 ) ;
#1586 = LINE ( 'NONE', #1041, #1195 ) ;
#1587 = CARTESIAN_POINT ( 'NONE',  ( -145.0000000000000284, -3.353798720221824946E-14, 42.49999999999999289 ) ) ;
#1588 = EDGE_CURVE ( 'NONE', #216, #1670, #507, .T. ) ;
#1589 = ORIENTED_EDGE ( 'NONE', *, *, #1544, .F. ) ;
#1590 = ORIENTED_EDGE ( 'NONE', *, *, #1893, .F. ) ;
#1591 = DIRECTION ( 'NONE',  ( 0.000000000000000000, -1.000000000000000000, 1.287488025362403787E-15 ) ) ;
#1592 = DIRECTION ( 'NONE',  ( 0.000000000000000000, 0.000000000000000000, -1.000000000000000000 ) ) ;
#1593 = FACE_BOUND ( 'NONE', #1819, .T. ) ;
#1594 = ORIENTED_EDGE ( 'NONE', *, *, #1331, .F. ) ;
#1595 = SURFACE_STYLE_FILL_AREA ( #916 ) ;
#1596 = EDGE_CURVE ( 'NONE', #1133, #1887, #566, .T. ) ;
#1597 = DIRECTION ( 'NONE',  ( -0.000000000000000000, 1.000000000000000000, -0.000000000000000000 ) ) ;
#1598 = CARTESIAN_POINT ( 'NONE',  ( 0.000000000000000000, 5.051668046482832750E-16, -4.000000000000000000 ) ) ;
#1599 = AXIS2_PLACEMENT_3D ( 'NONE', #1392, #1204, #1039 ) ;
#1600 = EDGE_LOOP ( 'NONE', ( #19, #148, #35, #864 ) ) ;
#1601 = ORIENTED_EDGE ( 'NONE', *, *, #1395, .F. ) ;
#1602 = CARTESIAN_POINT ( 'NONE',  ( -145.0000000000000284, -3.353798720221824946E-14, 47.50000000000000000 ) ) ;
#1603 = CARTESIAN_POINT ( 'NONE',  ( 145.0000000000000284, 2.993649167310367343, 45.00000000000000000 ) ) ;
#1604 = DIRECTION ( 'NONE',  ( 0.000000000000000000, 1.000000000000000000, -1.224646799147353207E-16 ) ) ;
#1605 = VECTOR ( 'NONE', #2165, 1000.000000000000000 ) ;
#1606 =( LENGTH_UNIT ( ) NAMED_UNIT ( * ) SI_UNIT ( .MILLI., .METRE. ) );
#1607 = ADVANCED_FACE ( 'NONE', ( #2071 ), #578, .T. ) ;
#1608 = CARTESIAN_POINT ( 'NONE',  ( -145.0000000000000284, 0.000000000000000000, -45.00000000000000000 ) ) ;
#1609 = PRODUCT_RELATED_PRODUCT_CATEGORY ( 'part', '', ( #118 ) ) ;
#1610 = EDGE_CURVE ( 'NONE', #2107, #860, #61, .T. ) ;
#1611 = ORIENTED_EDGE ( 'NONE', *, *, #359, .F. ) ;
#1612 =( REPRESENTATION_RELATIONSHIP ('NONE','NONE', #367, #354 ) REPRESENTATION_RELATIONSHIP_WITH_TRANSFORMATION ( #811 )SHAPE_REPRESENTATION_RELATIONSHIP( ) );
#1613 = ORIENTED_EDGE ( 'NONE', *, *, #2212, .T. ) ;
#1614 = PLANE ( 'NONE',  #570 ) ;
#1615 = FACE_OUTER_BOUND ( 'NONE', #843, .T. ) ;
#1617 = EDGE_LOOP ( 'NONE', ( #2222, #755, #815 ) ) ;
#1616 = CARTESIAN_POINT ( 'NONE',  ( 20.55500000000001748, 0.000000000000000000, 2.500000000000000888 ) ) ;
#1618 = VECTOR ( 'NONE', #2171, 1000.000000000000000 ) ;
#1619 = VECTOR ( 'NONE', #2007, 1000.000000000000000 ) ;
#1620 = VECTOR ( 'NONE', #1160, 1000.000000000000114 ) ;
#1621 = PRODUCT_DEFINITION_SHAPE ( 'NONE', 'NONE',  #453 ) ;
#1622 = FACE_OUTER_BOUND ( 'NONE', #2143, .T. ) ;
#1623 = DIRECTION ( 'NONE',  ( 0.000000000000000000, 0.000000000000000000, 1.000000000000000000 ) ) ;
#1624 = PRODUCT_CONTEXT ( 'NONE', #1085, 'mechanical' ) ;
#1625 = VERTEX_POINT ( 'NONE', #535 ) ;
#1626 = ORIENTED_EDGE ( 'NONE', *, *, #1168, .T. ) ;
#1627 = CARTESIAN_POINT ( 'NONE',  ( -157.0000000000000000, 10.00000000000000000, -56.99999999999997868 ) ) ;
#1628 = DIRECTION ( 'NONE',  ( -1.000000000000000000, 0.000000000000000000, -0.000000000000000000 ) ) ;
#1629 = ORIENTED_EDGE ( 'NONE', *, *, #180, .T. ) ;
#1631 = VERTEX_POINT ( 'NONE', #212 ) ;
#1630 = DIRECTION ( 'NONE',  ( -2.312964634635742957E-16, 0.000000000000000000, 1.000000000000000000 ) ) ;
#1632 = DIRECTION ( 'NONE',  ( -5.046468293750711010E-16, 1.000000000000000000, 0.000000000000000000 ) ) ;
#1633 = CARTESIAN_POINT ( 'NONE',  ( -31.74999999999995737, 0.000000000000000000, 0.000000000000000000 ) ) ;
#1634 = DIRECTION ( 'NONE',  ( -1.000000000000000000, -2.312964634635740985E-16, 0.000000000000000000 ) ) ;
#1635 = CIRCLE ( 'NONE', #1526, 2.649999999999985700 ) ;
#1636 = ORIENTED_EDGE ( 'NONE', *, *, #2015, .F. ) ;
#1637 = ORIENTED_EDGE ( 'NONE', *, *, #1473, .T. ) ;
#1638 = CIRCLE ( 'NONE', #1960, 2.649999999999985700 ) ;
#1639 = DIRECTION ( 'NONE',  ( -1.000000000000000000, 0.000000000000000000, -0.000000000000000000 ) ) ;
#1640 = DIRECTION ( 'NONE',  ( -1.000000000000000000, -0.000000000000000000, -0.000000000000000000 ) ) ;
#1641 = ORIENTED_EDGE ( 'NONE', *, *, #1992, .F. ) ;
#1642 = PRODUCT_DEFINITION ( 'UNKNOWN', '', #656, #1199 ) ;
#1644 = ORIENTED_EDGE ( 'NONE', *, *, #2194, .T. ) ;
#1643 = DIRECTION ( 'NONE',  ( -1.000000000000000000, -0.000000000000000000, -0.000000000000000000 ) ) ;
#1645 = CARTESIAN_POINT ( 'NONE',  ( 157.0000000000000000, 3.000000000000000000, 3.631354476378115974E-14 ) ) ;
#1646 = AXIS2_PLACEMENT_3D ( 'NONE', #1656, #1323, #77 ) ;
#1647 = FACE_OUTER_BOUND ( 'NONE', #950, .T. ) ;
#1648 = VECTOR ( 'NONE', #1186, 1000.000000000000000 ) ;
#1649 = VECTOR ( 'NONE', #1756, 1000.000000000000000 ) ;
#1650 = ORIENTED_EDGE ( 'NONE', *, *, #879, .T. ) ;
#1651 = CARTESIAN_POINT ( 'NONE',  ( 0.000000000000000000, 1.178949249685212974, -2.042000000000001148 ) ) ;
#1652 = ORIENTED_EDGE ( 'NONE', *, *, #2124, .F. ) ;
#1653 = CARTESIAN_POINT ( 'NONE',  ( 2.500000000000000000, -1.178949249685218748, -2.041999999999998039 ) ) ;
#1654 = DIRECTION ( 'NONE',  ( 0.000000000000000000, 0.4999999999999990008, -0.8660254037844391517 ) ) ;
#1655 = DIRECTION ( 'NONE',  ( 0.000000000000000000, 0.4999999999999990008, -0.8660254037844391517 ) ) ;
#1656 = CARTESIAN_POINT ( 'NONE',  ( 145.0000000000000284, 2.800000000000000266, 45.00000000000000000 ) ) ;
#1657 = MECHANICAL_DESIGN_GEOMETRIC_PRESENTATION_REPRESENTATION (  '', ( #2197 ), #1156 ) ;
#1658 = COLOUR_RGB ( '',0.8941176470588234615, 0.8941176470588234615, 0.8941176470588234615 ) ;
#1659 = ADVANCED_FACE ( 'NONE', ( #1061 ), #1948, .T. ) ;
#1660 = DIRECTION ( 'NONE',  ( 0.000000000000000000, 0.000000000000000000, 1.000000000000000000 ) ) ;
#1661 = VERTEX_POINT ( 'NONE', #1933 ) ;
#1662 = DIRECTION ( 'NONE',  ( 2.312964634635742957E-16, 0.000000000000000000, -1.000000000000000000 ) ) ;
#1663 = VERTEX_POINT ( 'NONE', #1240 ) ;
#1664 = LINE ( 'NONE', #112, #1648 ) ;
#1665 = CARTESIAN_POINT ( 'NONE',  ( 0.000000000000000000, -2.357898499370432166, 3.035766082959412415E-15 ) ) ;
#1666 = DIRECTION ( 'NONE',  ( 6.123233995736766036E-17, -1.000000000000000000, 0.000000000000000000 ) ) ;
#1667 = FACE_OUTER_BOUND ( 'NONE', #97, .T. ) ;
#1668 = EDGE_CURVE ( 'NONE', #1125, #625, #414, .T. ) ;
#1669 = AXIS2_PLACEMENT_3D ( 'NONE', #1205, #26, #883 ) ;
#1670 = VERTEX_POINT ( 'NONE', #202 ) ;
#1671 = DIRECTION ( 'NONE',  ( 1.000000000000000000, 2.312964634635740985E-16, 0.000000000000000000 ) ) ;
#1672 = VERTEX_POINT ( 'NONE', #1598 ) ;
#1673 = MANIFOLD_SOLID_BREP ( 'Tap Drill for M5 Tap2', #175 ) ;
#1674 = TOROIDAL_SURFACE ( 'NONE', #355, 2.700000000000000622, 0.2000000000000000111 ) ;
#1675 = DIRECTION ( 'NONE',  ( 0.000000000000000000, 0.000000000000000000, -1.000000000000000000 ) ) ;
#1676 = PLANE ( 'NONE',  #1904 ) ;
#1677 = EDGE_LOOP ( 'NONE', ( #1064, #761, #1695, #612 ) ) ;
#1678 = DIRECTION ( 'NONE',  ( 0.000000000000000000, 0.000000000000000000, -1.000000000000000000 ) ) ;
#1679 = DIRECTION ( 'NONE',  ( 0.000000000000000000, 0.000000000000000000, 1.000000000000000000 ) ) ;
#1680 = CIRCLE ( 'NONE', #1783, 0.1999999999999987899 ) ;
#1681 = EDGE_CURVE ( 'NONE', #830, #65, #193, .T. ) ;
#1682 = EDGE_LOOP ( 'NONE', ( #1903, #2190, #1778, #1468 ) ) ;
#1683 = DIRECTION ( 'NONE',  ( 0.000000000000000000, 0.000000000000000000, -1.000000000000000000 ) ) ;
#1684 = EDGE_LOOP ( 'NONE', ( #1375, #661, #1438, #1231 ) ) ;
#1685 = MANIFOLD_SOLID_BREP ( 'Hex', #290 ) ;
#1686 = MECHANICAL_DESIGN_GEOMETRIC_PRESENTATION_REPRESENTATION (  '', ( #1506 ), #972 ) ;
#1687 = CARTESIAN_POINT ( 'NONE',  ( -145.0000000000000284, -15.00000000000003197, -42.49999999999999289 ) ) ;
#1688 = PLANE ( 'NONE',  #777 ) ;
#1689 = ORIENTED_EDGE ( 'NONE', *, *, #819, .T. ) ;
#1690 = CARTESIAN_POINT ( 'NONE',  ( 145.0000000000000284, 0.000000000000000000, 45.00000000000000000 ) ) ;
#1691 = DIRECTION ( 'NONE',  ( 2.312964634635742957E-16, 0.000000000000000000, -1.000000000000000000 ) ) ;
#1692 = VECTOR ( 'NONE', #1201, 1000.000000000000000 ) ;
#1693 = VECTOR ( 'NONE', #770, 1000.000000000000000 ) ;
#1694 = AXIS2_PLACEMENT_3D ( 'NONE', #1405, #845, #674 ) ;
#1695 = ORIENTED_EDGE ( 'NONE', *, *, #373, .F. ) ;
#1696 = EDGE_LOOP ( 'NONE', ( #337, #1087, #1076, #1203 ) ) ;
#1697 = EDGE_CURVE ( 'NONE', #1316, #1670, #1070, .T. ) ;
#1698 = CARTESIAN_POINT ( 'NONE',  ( 2.500000000000000000, 2.357898499370431722, -2.818925648462311528E-15 ) ) ;
#1699 = CARTESIAN_POINT ( 'NONE',  ( 20.55500000000001748, 0.000000000000000000, 0.000000000000000000 ) ) ;
#1700 = VERTEX_POINT ( 'NONE', #120 ) ;
#1701 = CARTESIAN_POINT ( 'NONE',  ( -145.0000000000000284, 2.993649167310367343, -47.64999999999998437 ) ) ;
#1702 = CARTESIAN_POINT ( 'NONE',  ( -139.9999999999999716, -9.999999999999994671, 40.00000000000000000 ) ) ;
#1703 = DIRECTION ( 'NONE',  ( 6.123233995736766036E-17, -1.000000000000000000, 0.000000000000000000 ) ) ;
#1704 = VERTEX_POINT ( 'NONE', #1485 ) ;
#1705 = ADVANCED_FACE ( 'NONE', ( #1298 ), #450, .T. ) ;
#1706 = ORIENTED_EDGE ( 'NONE', *, *, #208, .F. ) ;
#1707 = EDGE_CURVE ( 'NONE', #1430, #1909, #63, .T. ) ;
#1708 = EDGE_CURVE ( 'NONE', #1569, #957, #799, .T. ) ;
#1709 = DIRECTION ( 'NONE',  ( 0.000000000000000000, 0.000000000000000000, -1.000000000000000000 ) ) ;
#1710 = DIRECTION ( 'NONE',  ( 0.000000000000000000, 0.000000000000000000, 1.000000000000000000 ) ) ;
#1711 = UNCERTAINTY_MEASURE_WITH_UNIT (LENGTH_MEASURE( 1.000000000000000082E-05 ), #428, 'distance_accuracy_value', 'NONE');
#1712 = EDGE_CURVE ( 'NONE', #1631, #776, #810, .T. ) ;
#1713 = ORIENTED_EDGE ( 'NONE', *, *, #1707, .F. ) ;
#1714 = DIRECTION ( 'NONE',  ( -0.000000000000000000, 1.000000000000000000, -0.000000000000000000 ) ) ;
#1715 = ORIENTED_EDGE ( 'NONE', *, *, #580, .T. ) ;
#1716 = ORIENTED_EDGE ( 'NONE', *, *, #381, .F. ) ;
#1717 = LINE ( 'NONE', #727, #2002 ) ;
#1718 = DIRECTION ( 'NONE',  ( -6.123233995736766036E-17, 1.000000000000000000, -0.000000000000000000 ) ) ;
#1719 = AXIS2_PLACEMENT_3D ( 'NONE', #1776, #413, #2152 ) ;
#1720 = DIRECTION ( 'NONE',  ( -0.000000000000000000, 1.000000000000000000, -0.000000000000000000 ) ) ;
#1721 = ADVANCED_FACE ( 'NONE', ( #615, #2140, #1132 ), #982, .T. ) ;
#1722 = ADVANCED_FACE ( 'NONE', ( #276 ), #2043, .T. ) ;
#1723 = PRESENTATION_LAYER_ASSIGNMENT (  '', '', ( #2197 ) ) ;
#1724 = AXIS2_PLACEMENT_3D ( 'NONE', #504, #153, #141 ) ;
#1725 = VERTEX_POINT ( 'NONE', #2008 ) ;
#1726 = AXIS2_PLACEMENT_3D ( 'NONE', #487, #1136, #1662 ) ;
#1727 = DIRECTION ( 'NONE',  ( 0.000000000000000000, -1.000000000000000000, 0.000000000000000000 ) ) ;
#1728 = DIRECTION ( 'NONE',  ( 0.000000000000000000, 0.000000000000000000, -1.000000000000000000 ) ) ;
#1729 = LINE ( 'NONE', #894, #1120 ) ;
#1730 = ADVANCED_FACE ( 'NONE', ( #1141 ), #1967, .T. ) ;
#1731 = CARTESIAN_POINT ( 'NONE',  ( -145.0000000000000284, 3.000000000000000000, -42.35000000000001563 ) ) ;
#1732 = CARTESIAN_POINT ( 'NONE',  ( 145.0000000000000284, 3.000000000000002665, -45.00000000000000000 ) ) ;
#1733 = ADVANCED_BREP_SHAPE_REPRESENTATION ( '', ( #1673, #30 ), #544 ) ;
#1734 = EDGE_CURVE ( 'NONE', #1133, #2144, #939, .T. ) ;
#1735 = VERTEX_POINT ( 'NONE', #1275 ) ;
#1736 = FACE_OUTER_BOUND ( 'NONE', #1244, .T. ) ;
#1737 = DIRECTION ( 'NONE',  ( -2.312964634635742957E-16, 0.000000000000000000, 1.000000000000000000 ) ) ;
#1738 = CARTESIAN_POINT ( 'NONE',  ( 2.500000000000000000, -1.178949249685218748, -2.041999999999998039 ) ) ;
#1739 = VECTOR ( 'NONE', #1654, 1000.000000000000114 ) ;
#1740 = EDGE_LOOP ( 'NONE', ( #1038, #1969, #68, #1028 ) ) ;
#1741 = LINE ( 'NONE', #392, #1878 ) ;
#1742 = TOROIDAL_SURFACE ( 'NONE', #1279, 2.700000000000000622, 0.2000000000000000111 ) ;
#1743 = CARTESIAN_POINT ( 'NONE',  ( -31.74999999999995737, 5.204748896376250699E-16, -4.250000000000000000 ) ) ;
#1744 = DIRECTION ( 'NONE',  ( 0.000000000000000000, 0.8660254037844380415, -0.5000000000000009992 ) ) ;
#1745 = ORIENTED_EDGE ( 'NONE', *, *, #1103, .T. ) ;
#1746 = VECTOR ( 'NONE', #603, 1000.000000000000000 ) ;
#1747 = ORIENTED_EDGE ( 'NONE', *, *, #868, .T. ) ;
#1748 = DIRECTION ( 'NONE',  ( 0.000000000000000000, 0.000000000000000000, -1.000000000000000000 ) ) ;
#1749 = CARTESIAN_POINT ( 'NONE',  ( -145.0000000000000284, -15.00000000000003197, 45.00000000000000000 ) ) ;
#1750 = DIRECTION ( 'NONE',  ( 0.000000000000000000, 0.000000000000000000, -1.000000000000000000 ) ) ;
#1751 = EDGE_CURVE ( 'NONE', #4, #1579, #1285, .T. ) ;
#1752 = CIRCLE ( 'NONE', #103, 0.2000000000000000944 ) ;
#1753 = CARTESIAN_POINT ( 'NONE',  ( -150.0000000000000000, 0.000000000000000000, 50.00000000000000000 ) ) ;
#1754 = CIRCLE ( 'NONE', #104, 2.500000000000002220 ) ;
#1755 = FACE_OUTER_BOUND ( 'NONE', #214, .T. ) ;
#1756 = DIRECTION ( 'NONE',  ( -0.000000000000000000, -0.000000000000000000, -1.000000000000000000 ) ) ;
#1757 = ORIENTED_EDGE ( 'NONE', *, *, #1344, .T. ) ;
#1758 = ORIENTED_EDGE ( 'NONE', *, *, #381, .T. ) ;
#1759 = DIRECTION ( 'NONE',  ( 0.000000000000000000, 0.000000000000000000, -1.000000000000000000 ) ) ;
#1760 = CARTESIAN_POINT ( 'NONE',  ( -139.9999999999999716, 2.312964634635743056E-15, -50.00000000000000000 ) ) ;
#1761 = DIRECTION ( 'NONE',  ( -0.000000000000000000, 1.287488025362403787E-15, 1.000000000000000000 ) ) ;
#1762 = EDGE_CURVE ( 'NONE', #833, #486, #772, .T. ) ;
#1763 = EDGE_LOOP ( 'NONE', ( #2058, #1979, #1032 ) ) ;
#1764 = DIRECTION ( 'NONE',  ( -1.000000000000000000, -0.000000000000000000, -0.000000000000000000 ) ) ;
#1765 = DIRECTION ( 'NONE',  ( 0.000000000000000000, 0.000000000000000000, 1.000000000000000000 ) ) ;
#1766 = ORIENTED_EDGE ( 'NONE', *, *, #1034, .T. ) ;
#1767 = EDGE_CURVE ( 'NONE', #1165, #575, #2148, .T. ) ;
#1768 = EDGE_LOOP ( 'NONE', ( #1290, #1124, #2128 ) ) ;
#1769 = LINE ( 'NONE', #1602, #675 ) ;
#1770 = DIRECTION ( 'NONE',  ( -0.000000000000000000, 0.000000000000000000, 1.000000000000000000 ) ) ;
#1771 = PLANE ( 'NONE',  #1123 ) ;
#1772 = EDGE_CURVE ( 'NONE', #833, #694, #263, .T. ) ;
#1773 = DIRECTION ( 'NONE',  ( 0.000000000000000000, 0.000000000000000000, -1.000000000000000000 ) ) ;
#1774 = AXIS2_PLACEMENT_3D ( 'NONE', #1539, #525, #1710 ) ;
#1775 = ADVANCED_FACE ( 'NONE', ( #1221 ), #1872, .F. ) ;
#1776 = CARTESIAN_POINT ( 'NONE',  ( 21.00000000000000355, 0.000000000000000000, 0.000000000000000000 ) ) ;
#1777 = CARTESIAN_POINT ( 'NONE',  ( -149.9999999999999716, -120.0000000000000142, 50.00000000000000000 ) ) ;
#1778 = ORIENTED_EDGE ( 'NONE', *, *, #1697, .T. ) ;
#1779 = ORIENTED_EDGE ( 'NONE', *, *, #2000, .F. ) ;
#1780 = DIRECTION ( 'NONE',  ( -0.000000000000000000, 1.000000000000000000, 1.224646799147353207E-16 ) ) ;
#1781 = CARTESIAN_POINT ( 'NONE',  ( 145.0000000000000284, 3.000000000000000000, 45.00000000000000000 ) ) ;
#1782 = DIRECTION ( 'NONE',  ( 0.000000000000000000, -0.000000000000000000, -1.000000000000000000 ) ) ;
#1783 = AXIS2_PLACEMENT_3D ( 'NONE', #1394, #1190, #1534 ) ;
#1784 = CARTESIAN_POINT ( 'NONE',  ( -145.0000000000000284, -15.00000000000003197, -45.00000000000000000 ) ) ;
#1785 = CARTESIAN_POINT ( 'NONE',  ( -160.0000000000000284, 10.00000000000000000, 60.00000000000001421 ) ) ;
#1786 = DIRECTION ( 'NONE',  ( 1.000000000000000000, 0.000000000000000000, 0.000000000000000000 ) ) ;
#1787 = AXIS2_PLACEMENT_3D ( 'NONE', #547, #1744, #11 ) ;
#1788 = EDGE_CURVE ( 'NONE', #1663, #1390, #1680, .T. ) ;
#1789 = ORIENTED_EDGE ( 'NONE', *, *, #1145, .F. ) ;
#1790 = EDGE_CURVE ( 'NONE', #415, #353, #2186, .T. ) ;
#1791 = ORIENTED_EDGE ( 'NONE', *, *, #2105, .F. ) ;
#1792 = CARTESIAN_POINT ( 'NONE',  ( 145.0000000000000284, 3.000000000000001776, 47.70000000000000284 ) ) ;
#1793 = LINE ( 'NONE', #210, #581 ) ;
#1794 = VERTEX_POINT ( 'NONE', #164 ) ;
#1796 = ORIENTED_EDGE ( 'NONE', *, *, #2000, .T. ) ;
#1795 = LINE ( 'NONE', #1238, #1892 ) ;
#1797 = DIRECTION ( 'NONE',  ( 0.000000000000000000, -1.287488025362403787E-15, -1.000000000000000000 ) ) ;
#1798 = CIRCLE ( 'NONE', #1223, 2.649999999999985700 ) ;
#1799 = VECTOR ( 'NONE', #992, 1000.000000000000000 ) ;
#1800 = FACE_BOUND ( 'NONE', #1864, .T. ) ;
#1801 = DIRECTION ( 'NONE',  ( 0.000000000000000000, 0.000000000000000000, 1.000000000000000000 ) ) ;
#1802 = EDGE_CURVE ( 'NONE', #1284, #1883, #719, .T. ) ;
#1803 = ORIENTED_EDGE ( 'NONE', *, *, #748, .F. ) ;
#1804 = EDGE_CURVE ( 'NONE', #1470, #1794, #139, .T. ) ;
#1805 = ORIENTED_EDGE ( 'NONE', *, *, #746, .F. ) ;
#1806 = FACE_OUTER_BOUND ( 'NONE', #1479, .T. ) ;
#1807 = FACE_OUTER_BOUND ( 'NONE', #1423, .T. ) ;
#1808 = EDGE_LOOP ( 'NONE', ( #1254, #1650, #1452, #195 ) ) ;
#1810 = ORIENTED_EDGE ( 'NONE', *, *, #144, .T. ) ;
#1809 = DIRECTION ( 'NONE',  ( 0.000000000000000000, -0.5000000000000013323, -0.8660254037844380415 ) ) ;
#1811 = FACE_OUTER_BOUND ( 'NONE', #1200, .T. ) ;
#1812 = DIRECTION ( 'NONE',  ( -6.123233995736766036E-17, 1.000000000000000000, -0.000000000000000000 ) ) ;
#1813 = AXIS2_PLACEMENT_3D ( 'NONE', #2051, #699, #1212 ) ;
#1814 = FILL_AREA_STYLE_COLOUR ( '', #404 ) ;
#1815 = ORIENTED_EDGE ( 'NONE', *, *, #1790, .F. ) ;
#1816 = VERTEX_POINT ( 'NONE', #1738 ) ;
#1817 = VECTOR ( 'NONE', #951, 1000.000000000000000 ) ;
#1818 = PLANE ( 'NONE',  #187 ) ;
#1819 = EDGE_LOOP ( 'NONE', ( #1111, #1352 ) ) ;
#1820 = PRODUCT_DEFINITION_SHAPE ( 'NONE', 'NONE',  #2233 ) ;
#1821 = DIRECTION ( 'NONE',  ( 0.000000000000000000, 0.000000000000000000, -1.000000000000000000 ) ) ;
#1822 = DIRECTION ( 'NONE',  ( 0.000000000000000000, 0.000000000000000000, -1.000000000000000000 ) ) ;
#1823 = ADVANCED_FACE ( 'NONE', ( #1667 ), #485, .T. ) ;
#1824 = LINE ( 'NONE', #638, #1019 ) ;
#1825 = DIRECTION ( 'NONE',  ( 2.312964634635742957E-16, -1.000000000000000000, 0.000000000000000000 ) ) ;
#1826 = AXIS2_PLACEMENT_3D ( 'NONE', #137, #668, #1821 ) ;
#1827 =( NAMED_UNIT ( * ) PLANE_ANGLE_UNIT ( ) SI_UNIT ( $, .RADIAN. ) );
#1828 = AXIS2_PLACEMENT_3D ( 'NONE', #1126, #268, #1639 ) ;
#1829 = ORIENTED_EDGE ( 'NONE', *, *, #1802, .F. ) ;
#1830 = CARTESIAN_POINT ( 'NONE',  ( 2.500000000000000000, -1.178949249685214307, 2.042000000000001592 ) ) ;
#1831 = VERTEX_POINT ( 'NONE', #1849 ) ;
#1832 = CARTESIAN_POINT ( 'NONE',  ( -150.0000000000000284, -9.999999999999994671, -40.00000000000000000 ) ) ;
#1833 = CARTESIAN_POINT ( 'NONE',  ( 20.55500000000001748, 3.061616997868384127E-16, -2.500000000000000888 ) ) ;
#1834 = CIRCLE ( 'NONE', #875, 2.649999999999985700 ) ;
#1835 = DIRECTION ( 'NONE',  ( 0.000000000000000000, -1.000000000000000000, 0.000000000000000000 ) ) ;
#1836 = CARTESIAN_POINT ( 'NONE',  ( 0.2500000000000002220, 0.000000000000000000, 0.000000000000000000 ) ) ;
#1837 = AXIS2_PLACEMENT_3D ( 'NONE', #949, #741, #2110 ) ;
#1838 = ITEM_DEFINED_TRANSFORMATION ( 'NONE', 'NONE', #1944,  #30 ) ;
#1839 = VECTOR ( 'NONE', #841, 1000.000000000000000 ) ;
#1840 = SURFACE_STYLE_FILL_AREA ( #1109 ) ;
#1841 = ORIENTED_EDGE ( 'NONE', *, *, #931, .F. ) ;
#1842 = CARTESIAN_POINT ( 'NONE',  ( -149.9999999999999716, -120.0000000000000142, 50.00000000000000000 ) ) ;
#1843 = ORIENTED_EDGE ( 'NONE', *, *, #1095, .T. ) ;
#1844 = DIRECTION ( 'NONE',  ( 0.000000000000000000, -0.000000000000000000, -1.000000000000000000 ) ) ;
#1845 = FACE_OUTER_BOUND ( 'NONE', #270, .T. ) ;
#1846 = ORIENTED_EDGE ( 'NONE', *, *, #1734, .T. ) ;
#1847 =( REPRESENTATION_RELATIONSHIP ('NONE','NONE', #367, #354 ) REPRESENTATION_RELATIONSHIP_WITH_TRANSFORMATION ( #2187 )SHAPE_REPRESENTATION_RELATIONSHIP( ) );
#1848 = CARTESIAN_POINT ( 'NONE',  ( -145.0000000000000284, -3.353798720221824946E-14, -47.50000000000000000 ) ) ;
#1849 = CARTESIAN_POINT ( 'NONE',  ( 2.500000000000000000, 1.768423874527823791, 1.020999999999998353 ) ) ;
#1850 = EDGE_CURVE ( 'NONE', #776, #1165, #895, .T. ) ;
#1851 = CARTESIAN_POINT ( 'NONE',  ( 0.000000000000000000, 0.000000000000000000, 0.000000000000000000 ) ) ;
#1852 = CONICAL_SURFACE ( 'NONE', #885, 2.500000000000002220, 1.029744258676654534 ) ;
#1853 = ORIENTED_EDGE ( 'NONE', *, *, #696, .F. ) ;
#1854 = PLANE ( 'NONE',  #71 ) ;
#1855 = ORIENTED_EDGE ( 'NONE', *, *, #1973, .F. ) ;
#1856 = VECTOR ( 'NONE', #192, 1000.000000000000000 ) ;
#1857 = CYLINDRICAL_SURFACE ( 'NONE', #976, 2.500000000000002220 ) ;
#1858 = LINE ( 'NONE', #1665, #1739 ) ;
#1859 = EDGE_LOOP ( 'NONE', ( #606, #667, #1879, #234 ) ) ;
#1860 = LINE ( 'NONE', #650, #759 ) ;
#1861 = CARTESIAN_POINT ( 'NONE',  ( 159.9999999999999716, 10.00000000000000000, 60.00000000000001421 ) ) ;
#1862 = CIRCLE ( 'NONE', #1460, 2.649999999999985700 ) ;
#1863 = CARTESIAN_POINT ( 'NONE',  ( 145.0000000000000284, 8.000000000000003553, -45.00000000000000000 ) ) ;
#1864 = EDGE_LOOP ( 'NONE', ( #2207, #6 ) ) ;
#1865 =( NAMED_UNIT ( * ) PLANE_ANGLE_UNIT ( ) SI_UNIT ( $, .RADIAN. ) );
#1866 = ORIENTED_EDGE ( 'NONE', *, *, #356, .T. ) ;
#1867 = CARTESIAN_POINT ( 'NONE',  ( -145.0000000000000284, 2.800000000000000266, 42.29999999999999716 ) ) ;
#1868 = DIRECTION ( 'NONE',  ( 1.000000000000000000, 0.000000000000000000, 0.000000000000000000 ) ) ;
#1869 = UNCERTAINTY_MEASURE_WITH_UNIT (LENGTH_MEASURE( 1.000000000000000082E-05 ), #1381, 'distance_accuracy_value', 'NONE');
#1870 = ORIENTED_EDGE ( 'NONE', *, *, #929, .T. ) ;
#1871 = CARTESIAN_POINT ( 'NONE',  ( 2.500000000000000000, -1.178949249685214307, 2.042000000000001592 ) ) ;
#1872 = PLANE ( 'NONE',  #286 ) ;
#1873 = SHAPE_REPRESENTATION_RELATIONSHIP ( 'NONE' , 'NONE' ,  #354, #1226 ) ;
#1874 = CIRCLE ( 'NONE', #2018, 2.041999999999999815 ) ;
#1875 = VECTOR ( 'NONE', #459, 1000.000000000000000 ) ;
#1876 = ADVANCED_FACE ( 'NONE', ( #1180 ), #2201, .T. ) ;
#1877 = EDGE_CURVE ( 'NONE', #1255, #848, #2077, .T. ) ;
#1878 = VECTOR ( 'NONE', #350, 1000.000000000000000 ) ;
#1879 = ORIENTED_EDGE ( 'NONE', *, *, #1272, .T. ) ;
#1880 = EDGE_LOOP ( 'NONE', ( #769, #975, #1981, #1936 ) ) ;
#1881 = CARTESIAN_POINT ( 'NONE',  ( -31.74999999999995737, 0.000000000000000000, 0.000000000000000000 ) ) ;
#1882 = DIRECTION ( 'NONE',  ( 0.000000000000000000, -1.000000000000000000, 0.000000000000000000 ) ) ;
#1883 = VERTEX_POINT ( 'NONE', #1702 ) ;
#1884 = LINE ( 'NONE', #1565, #1300 ) ;
#1885 = ORIENTED_EDGE ( 'NONE', *, *, #1802, .T. ) ;
#1886 = AXIS2_PLACEMENT_3D ( 'NONE', #2221, #198, #863 ) ;
#1887 = VERTEX_POINT ( 'NONE', #540 ) ;
#1888 = DIRECTION ( 'NONE',  ( -1.000000000000000000, -0.000000000000000000, -0.000000000000000000 ) ) ;
#1889 = CARTESIAN_POINT ( 'NONE',  ( 145.0000000000000284, 2.800000000000000266, 45.00000000000000000 ) ) ;
#1890 = ADVANCED_FACE ( 'NONE', ( #2091 ), #553, .F. ) ;
#1891 = DIRECTION ( 'NONE',  ( -0.000000000000000000, 1.000000000000000000, -0.000000000000000000 ) ) ;
#1892 = VECTOR ( 'NONE', #1809, 999.9999999999997726 ) ;
#1893 = EDGE_CURVE ( 'NONE', #848, #415, #1361, .T. ) ;
#1894 = AXIS2_PLACEMENT_3D ( 'NONE', #2109, #587, #1952 ) ;
#1895 = ORIENTED_EDGE ( 'NONE', *, *, #1877, .F. ) ;
#1896 = LINE ( 'NONE', #891, #91 ) ;
#1897 = DIRECTION ( 'NONE',  ( -1.000000000000000000, -6.123233995736766036E-17, -0.000000000000000000 ) ) ;
#1898 = EDGE_CURVE ( 'NONE', #1704, #1421, #1908, .T. ) ;
#1899 = DIRECTION ( 'NONE',  ( 0.000000000000000000, 0.5150380749100541555, 0.8571673007021122226 ) ) ;
#1900 = EDGE_CURVE ( 'NONE', #344, #1531, #1862, .T. ) ;
#1901 = CARTESIAN_POINT ( 'NONE',  ( -139.9999999999999716, -120.0000000000000142, 40.00000000000000000 ) ) ;
#1902 = VECTOR ( 'NONE', #1484, 1000.000000000000000 ) ;
#1903 = ORIENTED_EDGE ( 'NONE', *, *, #509, .T. ) ;
#1904 = AXIS2_PLACEMENT_3D ( 'NONE', #150, #2195, #1822 ) ;
#1905 = VECTOR ( 'NONE', #764, 1000.000000000000114 ) ;
#1906 = DIRECTION ( 'NONE',  ( 0.000000000000000000, 0.000000000000000000, -1.000000000000000000 ) ) ;
#1907 = LINE ( 'NONE', #170, #88 ) ;
#1908 = LINE ( 'NONE', #2021, #1570 ) ;
#1909 = VERTEX_POINT ( 'NONE', #1056 ) ;
#1910 = CARTESIAN_POINT ( 'NONE',  ( -145.0000000000000284, -16.50215154756893554, -45.00000000000000000 ) ) ;
#1911 = CARTESIAN_POINT ( 'NONE',  ( 156.9999999999999716, 10.00000000000000000, 57.00000000000000711 ) ) ;
#1912 = DIRECTION ( 'NONE',  ( -5.046468293750711010E-16, 1.000000000000000000, 0.000000000000000000 ) ) ;
#1913 =( REPRESENTATION_RELATIONSHIP ('NONE','NONE', #367, #38 ) REPRESENTATION_RELATIONSHIP_WITH_TRANSFORMATION ( #1838 )SHAPE_REPRESENTATION_RELATIONSHIP( ) );
#1914 = ORIENTED_EDGE ( 'NONE', *, *, #1681, .T. ) ;
#1915 = ORIENTED_EDGE ( 'NONE', *, *, #482, .F. ) ;
#1916 = LINE ( 'NONE', #882, #461 ) ;
#1917 = CARTESIAN_POINT ( 'NONE',  ( -145.0000000000000284, -15.00000000000003197, 45.00000000000000000 ) ) ;
#1918 = CARTESIAN_POINT ( 'NONE',  ( 2.500000000000000000, -1.178949249685214307, 2.042000000000001592 ) ) ;
#1919 = AXIS2_PLACEMENT_3D ( 'NONE', #2027, #660, #2172 ) ;
#1920 = DIRECTION ( 'NONE',  ( 2.312964634635742957E-16, -1.000000000000000000, 0.000000000000000000 ) ) ;
#1921 = CARTESIAN_POINT ( 'NONE',  ( 156.9999999999999716, 10.00000000000000000, 57.00000000000000711 ) ) ;
#1922 = FILL_AREA_STYLE_COLOUR ( '', #291 ) ;
#1923 = EDGE_CURVE ( 'NONE', #1661, #1439, #199, .T. ) ;
#1924 = EDGE_LOOP ( 'NONE', ( #751, #1334, #1559, #2064 ) ) ;
#1925 = ORIENTED_EDGE ( 'NONE', *, *, #1007, .T. ) ;
#1926 = FACE_OUTER_BOUND ( 'NONE', #440, .T. ) ;
#1927 = DIRECTION ( 'NONE',  ( -1.000000000000000000, 0.000000000000000000, -0.000000000000000000 ) ) ;
#1928 = FACE_BOUND ( 'NONE', #2047, .T. ) ;
#1929 = ORIENTED_EDGE ( 'NONE', *, *, #356, .F. ) ;
#1930 = VECTOR ( 'NONE', #325, 1000.000000000000000 ) ;
#1931 = DIRECTION ( 'NONE',  ( 6.123233995736766036E-17, -1.000000000000000000, 0.000000000000000000 ) ) ;
#1932 = AXIS2_PLACEMENT_3D ( 'NONE', #614, #1986, #1131 ) ;
#1933 = CARTESIAN_POINT ( 'NONE',  ( 159.9999999999999716, 10.00000000000000000, 60.00000000000001421 ) ) ;
#1934 = ADVANCED_FACE ( 'NONE', ( #154 ), #27, .F. ) ;
#1935 = EDGE_CURVE ( 'NONE', #1625, #575, #1234, .T. ) ;
#1936 = ORIENTED_EDGE ( 'NONE', *, *, #1309, .F. ) ;
#1937 = ADVANCED_FACE ( 'NONE', ( #1943, #913, #1113, #1928, #1593 ), #48, .F. ) ;
#1938 = CIRCLE ( 'NONE', #67, 2.649999999999985700 ) ;
#1939 = ORIENTED_EDGE ( 'NONE', *, *, #2166, .F. ) ;
#1940 = DIRECTION ( 'NONE',  ( 6.123233995736766036E-17, -1.000000000000000000, 0.000000000000000000 ) ) ;
#1941 = ADVANCED_FACE ( 'NONE', ( #588 ), #925, .F. ) ;
#1942 = DIRECTION ( 'NONE',  ( 0.000000000000000000, 0.000000000000000000, -1.000000000000000000 ) ) ;
#1943 = FACE_OUTER_BOUND ( 'NONE', #1382, .T. ) ;
#1944 = AXIS2_PLACEMENT_3D ( 'NONE', #2045, #185, #342 ) ;
#1945 = CIRCLE ( 'NONE', #986, 0.1999999999999987899 ) ;
#1946 = LINE ( 'NONE', #412, #517 ) ;
#1947 = CARTESIAN_POINT ( 'NONE',  ( -139.9999999999999716, -120.0000000000000142, -40.00000000000000000 ) ) ;
#1948 = PLANE ( 'NONE',  #437 ) ;
#1949 = ORIENTED_EDGE ( 'NONE', *, *, #165, .F. ) ;
#1950 = ORIENTED_EDGE ( 'NONE', *, *, #765, .T. ) ;
#1951 = DIRECTION ( 'NONE',  ( 0.000000000000000000, 0.000000000000000000, -1.000000000000000000 ) ) ;
#1952 = DIRECTION ( 'NONE',  ( 0.000000000000000000, 0.5000000000000011102, 0.8660254037844379305 ) ) ;
#1953 = CARTESIAN_POINT ( 'NONE',  ( 5.000000000000000888, 0.000000000000000000, 0.000000000000000000 ) ) ;
#1954 = DIRECTION ( 'NONE',  ( -1.000000000000000000, -0.000000000000000000, -0.000000000000000000 ) ) ;
#1955 = AXIS2_PLACEMENT_3D ( 'NONE', #1393, #1942, #69 ) ;
#1956 = EDGE_CURVE ( 'NONE', #1165, #1631, #563, .T. ) ;
#1957 = DIRECTION ( 'NONE',  ( 0.000000000000000000, 0.000000000000000000, 1.000000000000000000 ) ) ;
#1958 = CARTESIAN_POINT ( 'NONE',  ( 0.2500000000000002220, 0.000000000000000000, 0.000000000000000000 ) ) ;
#1959 = ADVANCED_FACE ( 'NONE', ( #238 ), #390, .F. ) ;
#1960 = AXIS2_PLACEMENT_3D ( 'NONE', #1415, #697, #1748 ) ;
#1961 = APPLICATION_PROTOCOL_DEFINITION ( 'draft international standard', 'automotive_design', 1998, #849 ) ;
#1962 = PRODUCT ( 'tray', 'tray', '', ( #1449 ) ) ;
#1963 = VERTEX_POINT ( 'NONE', #574 ) ;
#1964 = EDGE_LOOP ( 'NONE', ( #728, #1218, #1000 ) ) ;
#1965 = LINE ( 'NONE', #573, #1096 ) ;
#1966 = DIRECTION ( 'NONE',  ( -1.000000000000000000, -0.000000000000000000, -0.000000000000000000 ) ) ;
#1967 = TOROIDAL_SURFACE ( 'NONE', #2224, 4.000000000000000000, 0.2500000000000000000 ) ;
#1969 = ORIENTED_EDGE ( 'NONE', *, *, #703, .F. ) ;
#1968 = CARTESIAN_POINT ( 'NONE',  ( -31.74999999999995737, 0.000000000000000000, 2.500000000000000444 ) ) ;
#1970 = EDGE_CURVE ( 'NONE', #835, #256, #1793, .T. ) ;
#1971 = CARTESIAN_POINT ( 'NONE',  ( -145.0000000000000284, 2.800000000000000266, 47.70000000000000284 ) ) ;
#1972 = DIRECTION ( 'NONE',  ( -2.312964634635742957E-16, -0.000000000000000000, 1.000000000000000000 ) ) ;
#1973 = EDGE_CURVE ( 'NONE', #1794, #627, #444, .T. ) ;
#1974 = DIRECTION ( 'NONE',  ( -1.000000000000000000, -0.000000000000000000, -0.000000000000000000 ) ) ;
#1975 = ORIENTED_EDGE ( 'NONE', *, *, #1168, .F. ) ;
#1976 = ORIENTED_EDGE ( 'NONE', *, *, #1422, .F. ) ;
#1977 = DIRECTION ( 'NONE',  ( 1.000000000000000000, 0.000000000000000000, 0.000000000000000000 ) ) ;
#1978 = LINE ( 'NONE', #2180, #34 ) ;
#1979 = ORIENTED_EDGE ( 'NONE', *, *, #1344, .F. ) ;
#1981 = ORIENTED_EDGE ( 'NONE', *, *, #180, .F. ) ;
#1980 = CARTESIAN_POINT ( 'NONE',  ( -31.74999999999995737, 3.061616997868383634E-16, -2.500000000000000444 ) ) ;
#1982 = FACE_OUTER_BOUND ( 'NONE', #417, .T. ) ;
#1983 = AXIS2_PLACEMENT_3D ( 'NONE', #73, #936, #768 ) ;
#1984 = CIRCLE ( 'NONE', #1161, 4.000000000000000000 ) ;
#1985 = VECTOR ( 'NONE', #1327, 1000.000000000000000 ) ;
#1986 = DIRECTION ( 'NONE',  ( 1.000000000000000000, 0.000000000000000000, 0.000000000000000000 ) ) ;
#1987 = DIRECTION ( 'NONE',  ( 0.000000000000000000, 0.4999999999999990008, -0.8660254037844391517 ) ) ;
#1988 = APPLICATION_PROTOCOL_DEFINITION ( 'draft international standard', 'automotive_design', 1998, #2073 ) ;
#1989 = ORIENTED_EDGE ( 'NONE', *, *, #1473, .F. ) ;
#1990 = ORIENTED_EDGE ( 'NONE', *, *, #541, .T. ) ;
#1991 = DIRECTION ( 'NONE',  ( 0.000000000000000000, -0.4999999999999993339, 0.8660254037844390407 ) ) ;
#1992 = EDGE_CURVE ( 'NONE', #1348, #957, #1455, .T. ) ;
#1993 = EDGE_LOOP ( 'NONE', ( #1853, #1017, #568, #81 ) ) ;
#1994 = PLANE ( 'NONE',  #1321 ) ;
#1995 = DIRECTION ( 'NONE',  ( 0.000000000000000000, -0.4999999999999993339, 0.8660254037844390407 ) ) ;
#1996 = LINE ( 'NONE', #2214, #1261 ) ;
#1997 =( NAMED_UNIT ( * ) PLANE_ANGLE_UNIT ( ) SI_UNIT ( $, .RADIAN. ) );
#1998 = CONTEXT_DEPENDENT_SHAPE_REPRESENTATION ( #1612, #462 ) ;
#1999 = SURFACE_SIDE_STYLE ('',( #1840 ) ) ;
#2000 = EDGE_CURVE ( 'NONE', #627, #226, #1340, .T. ) ;
#2001 = EDGE_LOOP ( 'NONE', ( #1248, #716 ) ) ;
#2002 = VECTOR ( 'NONE', #1030, 1000.000000000000114 ) ;
#2003 = CARTESIAN_POINT ( 'NONE',  ( -150.0000000000000284, -9.999999999999994671, 40.00000000000000000 ) ) ;
#2004 = ORIENTED_EDGE ( 'NONE', *, *, #1788, .T. ) ;
#2005 = FACE_OUTER_BOUND ( 'NONE', #1481, .T. ) ;
#2006 = CARTESIAN_POINT ( 'NONE',  ( -149.9999999999999716, -120.0000000000000142, 40.00000000000000000 ) ) ;
#2007 = DIRECTION ( 'NONE',  ( -1.000000000000000000, -0.000000000000000000, -0.000000000000000000 ) ) ;
#2008 = CARTESIAN_POINT ( 'NONE',  ( 145.0000000000000284, 0.000000000000000000, -42.35000000000001563 ) ) ;
#2009 = SHAPE_REPRESENTATION_RELATIONSHIP ( 'NONE' , 'NONE' ,  #38, #1733 ) ;
#2010 = VECTOR ( 'NONE', #1578, 1000.000000000000000 ) ;
#2011 = ADVANCED_FACE ( 'NONE', ( #1615 ), #726, .T. ) ;
#2012 = ORIENTED_EDGE ( 'NONE', *, *, #2122, .F. ) ;
#2013 = CARTESIAN_POINT ( 'NONE',  ( 156.9999999999999716, 10.00000000000000000, 60.00000000000001421 ) ) ;
#2014 = EDGE_LOOP ( 'NONE', ( #235, #308 ) ) ;
#2015 = EDGE_CURVE ( 'NONE', #2192, #405, #840, .T. ) ;
#2016 = FACE_BOUND ( 'NONE', #802, .T. ) ;
#2017 = DIRECTION ( 'NONE',  ( 0.000000000000000000, 0.000000000000000000, 1.000000000000000000 ) ) ;
#2018 = AXIS2_PLACEMENT_3D ( 'NONE', #464, #1640, #1342 ) ;
#2019 = ORIENTED_EDGE ( 'NONE', *, *, #1900, .F. ) ;
#2020 = DIRECTION ( 'NONE',  ( 0.000000000000000000, 0.000000000000000000, -1.000000000000000000 ) ) ;
#2021 = CARTESIAN_POINT ( 'NONE',  ( -2.471980953266949321E-15, 10.00000000000000000, -56.99999999999998579 ) ) ;
#2022 = AXIS2_PLACEMENT_3D ( 'NONE', #1258, #1604, #1583 ) ;
#2023 = ORIENTED_EDGE ( 'NONE', *, *, #993, .T. ) ;
#2024 = LINE ( 'NONE', #834, #1553 ) ;
#2025 = EDGE_LOOP ( 'NONE', ( #1815, #1590, #1144, #1601 ) ) ;
#2026 = LINE ( 'NONE', #2050, #1618 ) ;
#2027 = CARTESIAN_POINT ( 'NONE',  ( 21.00000000000000355, 0.000000000000000000, 0.000000000000000000 ) ) ;
#2028 = ORIENTED_EDGE ( 'NONE', *, *, #467, .F. ) ;
#2029 = CARTESIAN_POINT ( 'NONE',  ( 2.500000000000000000, 2.629050547790028946E-15, 2.042000000000000259 ) ) ;
#2030 = DIRECTION ( 'NONE',  ( 0.000000000000000000, 0.000000000000000000, -1.000000000000000000 ) ) ;
#2031 = DIRECTION ( 'NONE',  ( 6.123233995736766036E-17, -1.000000000000000000, 0.000000000000000000 ) ) ;
#2032 = VECTOR ( 'NONE', #1995, 1000.000000000000000 ) ;
#2033 = ORIENTED_EDGE ( 'NONE', *, *, #1877, .T. ) ;
#2034 =( NAMED_UNIT ( * ) SI_UNIT ( $, .STERADIAN. ) SOLID_ANGLE_UNIT ( ) );
#2035 = EDGE_LOOP ( 'NONE', ( #2023, #909 ) ) ;
#2036 =( REPRESENTATION_RELATIONSHIP ('NONE','NONE', #367, #354 ) REPRESENTATION_RELATIONSHIP_WITH_TRANSFORMATION ( #630 )SHAPE_REPRESENTATION_RELATIONSHIP( ) );
#2037 = AXIS2_PLACEMENT_3D ( 'NONE', #189, #207, #1581 ) ;
#2038 = CARTESIAN_POINT ( 'NONE',  ( -145.0000000000000284, 2.993649167310367343, 45.00000000000000000 ) ) ;
#2039 = CARTESIAN_POINT ( 'NONE',  ( -150.0000000000000284, -9.999999999999994671, 40.00000000000000000 ) ) ;
#2040 = ORIENTED_EDGE ( 'NONE', *, *, #1241, .F. ) ;
#2041 = CARTESIAN_POINT ( 'NONE',  ( -149.9999999999999716, -120.0000000000000142, 50.00000000000000000 ) ) ;
#2042 = CARTESIAN_POINT ( 'NONE',  ( 159.9999999999999716, 0.000000000000000000, 60.00000000000001421 ) ) ;
#2043 = TOROIDAL_SURFACE ( 'NONE', #1646, 2.700000000000000622, 0.2000000000000000111 ) ;
#2044 = PRODUCT_RELATED_PRODUCT_CATEGORY ( 'part', '', ( #967 ) ) ;
#2045 = CARTESIAN_POINT ( 'NONE',  ( 0.000000000000000000, 0.000000000000000000, 0.000000000000000000 ) ) ;
#2046 = CIRCLE ( 'NONE', #1826, 2.700000000000001066 ) ;
#2047 = EDGE_LOOP ( 'NONE', ( #178, #1086 ) ) ;
#2048 = VECTOR ( 'NONE', #1977, 1000.000000000000000 ) ;
#2049 = ORIENTED_EDGE ( 'NONE', *, *, #266, .T. ) ;
#2050 = CARTESIAN_POINT ( 'NONE',  ( 2.500000000000000000, -2.357898499370432166, 3.035766082959412415E-15 ) ) ;
#2051 = CARTESIAN_POINT ( 'NONE',  ( 2.500000000000000000, 2.357898499370431722, -2.818925648462311528E-15 ) ) ;
#2052 = PRODUCT_DEFINITION_CONTEXT ( 'detailed design', #431, 'design' ) ;
#2053 = VERTEX_POINT ( 'NONE', #1292 ) ;
#2054 = CARTESIAN_POINT ( 'NONE',  ( -145.0000000000000284, -3.353798720221824946E-14, -42.49999999999999289 ) ) ;
#2055 = DIRECTION ( 'NONE',  ( 0.000000000000000000, 0.000000000000000000, 1.000000000000000000 ) ) ;
#2056 = CIRCLE ( 'NONE', #182, 0.1999999999999987899 ) ;
#2057 = CIRCLE ( 'NONE', #1264, 2.500000000000000888 ) ;
#2058 = ORIENTED_EDGE ( 'NONE', *, *, #670, .T. ) ;
#2059 = ORIENTED_EDGE ( 'NONE', *, *, #1712, .T. ) ;
#2060 = DIRECTION ( 'NONE',  ( -1.000000000000000000, -0.000000000000000000, -0.000000000000000000 ) ) ;
#2061 = ADVANCED_FACE ( 'NONE', ( #83 ), #754, .T. ) ;
#2062 = DIRECTION ( 'NONE',  ( -5.046468293750711010E-16, 1.000000000000000000, 0.000000000000000000 ) ) ;
#2063 = CARTESIAN_POINT ( 'NONE',  ( -139.9999999999999716, -120.0000000000000142, 50.00000000000000000 ) ) ;
#2064 = ORIENTED_EDGE ( 'NONE', *, *, #1092, .F. ) ;
#2065 = AXIS2_PLACEMENT_3D ( 'NONE', #608, #731, #1592 ) ;
#2066 = ORIENTED_EDGE ( 'NONE', *, *, #1143, .T. ) ;
#2067 = EDGE_CURVE ( 'NONE', #60, #396, #659, .T. ) ;
#2068 = CARTESIAN_POINT ( 'NONE',  ( 5.000000000000000888, 0.000000000000000000, 0.000000000000000000 ) ) ;
#2069 = LINE ( 'NONE', #1220, #557 ) ;
#2070 = CARTESIAN_POINT ( 'NONE',  ( -145.0000000000000284, -3.358697307418414604E-14, -42.49999999999999289 ) ) ;
#2071 = FACE_OUTER_BOUND ( 'NONE', #1364, .T. ) ;
#2072 = VECTOR ( 'NONE', #1014, 1000.000000000000000 ) ;
#2073 = APPLICATION_CONTEXT ( 'automotive_design' ) ;
#2074 = ORIENTED_EDGE ( 'NONE', *, *, #823, .T. ) ;
#2075 = CARTESIAN_POINT ( 'NONE',  ( 145.0000000000000284, 3.000000000000000000, -45.00000000000000000 ) ) ;
#2076 = DIRECTION ( 'NONE',  ( 0.000000000000000000, 0.000000000000000000, -1.000000000000000000 ) ) ;
#2077 = LINE ( 'NONE', #494, #712 ) ;
#2078 = AXIS2_PLACEMENT_3D ( 'NONE', #2082, #383, #887 ) ;
#2079 = ORIENTED_EDGE ( 'NONE', *, *, #1092, .T. ) ;
#2080 = CARTESIAN_POINT ( 'NONE',  ( -145.0000000000000284, 2.800000000000000266, -42.29999999999999716 ) ) ;
#2081 = CYLINDRICAL_SURFACE ( 'NONE', #1, 2.500000000000000444 ) ;
#2082 = CARTESIAN_POINT ( 'NONE',  ( -145.0000000000000284, -3.358697307418414604E-14, -45.00000000000000000 ) ) ;
#2083 = EDGE_CURVE ( 'NONE', #1625, #1165, #666, .T. ) ;
#2084 = AXIS2_PLACEMENT_3D ( 'NONE', #865, #904, #1227 ) ;
#2085 = EDGE_LOOP ( 'NONE', ( #1626, #136, #515, #1177 ) ) ;
#2086 = VECTOR ( 'NONE', #743, 1000.000000000000114 ) ;
#2087 = AXIS2_PLACEMENT_3D ( 'NONE', #253, #39, #1442 ) ;
#2088 = EDGE_LOOP ( 'NONE', ( #1046, #1689, #2040, #1716 ) ) ;
#2089 = CARTESIAN_POINT ( 'NONE',  ( 2.500000000000000000, 2.357898499370431722, -2.818925648462311528E-15 ) ) ;
#2090 = LINE ( 'NONE', #1048, #527 ) ;
#2091 = FACE_OUTER_BOUND ( 'NONE', #1525, .T. ) ;
#2092 = CARTESIAN_POINT ( 'NONE',  ( 21.00000000000000355, 0.000000000000000000, 0.000000000000000000 ) ) ;
#2093 = ADVANCED_FACE ( 'NONE', ( #732 ), #1771, .F. ) ;
#2094 = CARTESIAN_POINT ( 'NONE',  ( -145.0000000000000284, 3.000000000000001776, 47.70000000000000284 ) ) ;
#2095 = SURFACE_SIDE_STYLE ('',( #725 ) ) ;
#2096 = ORIENTED_EDGE ( 'NONE', *, *, #744, .F. ) ;
#2097 = ORIENTED_EDGE ( 'NONE', *, *, #1573, .F. ) ;
#2098 = CARTESIAN_POINT ( 'NONE',  ( -150.0000000000000000, 0.000000000000000000, -50.00000000000000000 ) ) ;
#2099 = CARTESIAN_POINT ( 'NONE',  ( 4.999999999999997335, 0.000000000000000000, 0.000000000000000000 ) ) ;
#2100 = PLANE ( 'NONE',  #156 ) ;
#2101 = DIRECTION ( 'NONE',  ( 0.000000000000000000, 0.000000000000000000, 1.000000000000000000 ) ) ;
#2102 = AXIS2_PLACEMENT_3D ( 'NONE', #739, #2118, #923 ) ;
#2103 = ADVANCED_FACE ( 'NONE', ( #1417 ), #2100, .F. ) ;
#2104 = DIRECTION ( 'NONE',  ( 0.000000000000000000, -1.000000000000000000, 0.000000000000000000 ) ) ;
#2105 = EDGE_CURVE ( 'NONE', #1704, #44, #70, .T. ) ;
#2106 = ORIENTED_EDGE ( 'NONE', *, *, #1492, .T. ) ;
#2107 = VERTEX_POINT ( 'NONE', #474 ) ;
#2108 = CARTESIAN_POINT ( 'NONE',  ( -145.0000000000000284, 2.800000000000000266, 45.00000000000000000 ) ) ;
#2109 = CARTESIAN_POINT ( 'NONE',  ( 2.500000000000000000, 2.357898499370431722, -2.818925648462311528E-15 ) ) ;
#2110 = DIRECTION ( 'NONE',  ( 0.000000000000000000, 0.000000000000000000, 1.000000000000000000 ) ) ;
#2111 = CLOSED_SHELL ( 'NONE', ( #1722, #946, #352, #345, #2204, #1934, #1214, #146, #1397, #287, #941, #305, #1937, #66, #423, #1959, #2129, #2093, #1472, #2173, #1107, #1659, #1299, #246, #2011, #171, #1239 ) ) ;
#2112 = SURFACE_STYLE_USAGE ( .BOTH. , #599 ) ;
#2113 = VECTOR ( 'NONE', #1597, 1000.000000000000000 ) ;
#2114 = FACE_OUTER_BOUND ( 'NONE', #1012, .T. ) ;
#2115 = CARTESIAN_POINT ( 'NONE',  ( 0.2500000000000002220, 5.204748896376250699E-16, -4.250000000000000000 ) ) ;
#2116 = CIRCLE ( 'NONE', #2084, 2.649999999999985700 ) ;
#2117 = ORIENTED_EDGE ( 'NONE', *, *, #823, .F. ) ;
#2118 = DIRECTION ( 'NONE',  ( -0.000000000000000000, 1.000000000000000000, -0.000000000000000000 ) ) ;
#2119 = DIRECTION ( 'NONE',  ( 1.000000000000000000, 0.000000000000000000, 0.000000000000000000 ) ) ;
#2120 = DIRECTION ( 'NONE',  ( 0.000000000000000000, -1.000000000000000000, 0.000000000000000000 ) ) ;
#2121 = AXIS2_PLACEMENT_3D ( 'NONE', #1090, #902, #434 ) ;
#2122 = EDGE_CURVE ( 'NONE', #1505, #957, #1978, .T. ) ;
#2123 = AXIS2_PLACEMENT_3D ( 'NONE', #1187, #1868, #468 ) ;
#2124 = EDGE_CURVE ( 'NONE', #805, #643, #2024, .T. ) ;
#2125 = DIRECTION ( 'NONE',  ( 1.000000000000000000, 6.123233995736766036E-17, -1.224646799147353207E-16 ) ) ;
#2126 = DIRECTION ( 'NONE',  ( -0.000000000000000000, 1.000000000000000000, -0.000000000000000000 ) ) ;
#2127 = CARTESIAN_POINT ( 'NONE',  ( 2.500000000000000000, -2.357898499370432166, 3.035766082959412415E-15 ) ) ;
#2128 = ORIENTED_EDGE ( 'NONE', *, *, #2212, .F. ) ;
#2129 = ADVANCED_FACE ( 'NONE', ( #1807 ), #109, .F. ) ;
#2130 = ORIENTED_EDGE ( 'NONE', *, *, #1236, .T. ) ;
#2131 = CARTESIAN_POINT ( 'NONE',  ( -160.0000000000000000, 0.000000000000000000, -59.99999999999998579 ) ) ;
#2132 = CARTESIAN_POINT ( 'NONE',  ( 156.9999999999999432, 10.00000000000000000, -56.99999999999999289 ) ) ;
#2133 = EDGE_CURVE ( 'NONE', #643, #1057, #124, .T. ) ;
#2135 = EDGE_LOOP ( 'NONE', ( #1855, #54, #503, #1779 ) ) ;
#2134 = LINE ( 'NONE', #1294, #742 ) ;
#2136 = DIRECTION ( 'NONE',  ( 0.000000000000000000, 0.000000000000000000, 1.000000000000000000 ) ) ;
#2137 = CIRCLE ( 'NONE', #1488, 0.2000000000000000944 ) ;
#2138 = ADVANCED_BREP_SHAPE_REPRESENTATION ( '', ( #969, #30 ), #1049 ) ;
#2139 = CARTESIAN_POINT ( 'NONE',  ( -145.0000000000000284, 0.000000000000000000, 47.64999999999998437 ) ) ;
#2140 = FACE_BOUND ( 'NONE', #930, .T. ) ;
#2141 = CIRCLE ( 'NONE', #496, 2.500000000000002220 ) ;
#2142 = ITEM_DEFINED_TRANSFORMATION ( 'NONE', 'NONE', #113,  #30 ) ;
#2143 = EDGE_LOOP ( 'NONE', ( #475, #1414, #774 ) ) ;
#2144 = VERTEX_POINT ( 'NONE', #1171 ) ;
#2145 = LINE ( 'NONE', #1246, #2048 ) ;
#2146 = DIRECTION ( 'NONE',  ( -1.000000000000000000, -0.000000000000000000, -0.000000000000000000 ) ) ;
#2147 = ORIENTED_EDGE ( 'NONE', *, *, #334, .F. ) ;
#2148 = CIRCLE ( 'NONE', #1250, 2.041999999999999815 ) ;
#2150 = ORIENTED_EDGE ( 'NONE', *, *, #1668, .F. ) ;
#2149 = CARTESIAN_POINT ( 'NONE',  ( -139.9999999999999716, -120.0000000000000142, 50.00000000000000000 ) ) ;
#2151 = DIRECTION ( 'NONE',  ( -0.000000000000000000, 1.000000000000000000, -0.000000000000000000 ) ) ;
#2152 = DIRECTION ( 'NONE',  ( 0.000000000000000000, 0.000000000000000000, 1.000000000000000000 ) ) ;
#2153 = ADVANCED_FACE ( 'NONE', ( #623 ), #1818, .T. ) ;
#2154 = FILL_AREA_STYLE ('',( #131 ) ) ;
#2155 = ORIENTED_EDGE ( 'NONE', *, *, #734, .T. ) ;
#2156 = VERTEX_POINT ( 'NONE', #309 ) ;
#2157 = LINE ( 'NONE', #1651, #255 ) ;
#2158 = ORIENTED_EDGE ( 'NONE', *, *, #2196, .T. ) ;
#2160 = ORIENTED_EDGE ( 'NONE', *, *, #1095, .F. ) ;
#2159 = CARTESIAN_POINT ( 'NONE',  ( 159.9999999999999716, 10.00000000000000000, 60.00000000000001421 ) ) ;
#2161 = AXIS2_PLACEMENT_3D ( 'NONE', #1146, #323, #1504 ) ;
#2162 = DIRECTION ( 'NONE',  ( -0.000000000000000000, 1.000000000000000000, -0.000000000000000000 ) ) ;
#2163 = AXIS2_PLACEMENT_3D ( 'NONE', #1971, #2125, #613 ) ;
#2164 = PRODUCT_DEFINITION_SHAPE ( 'NONE', 'NONE',  #2229 ) ;
#2165 = DIRECTION ( 'NONE',  ( -0.000000000000000000, 1.000000000000000000, -0.000000000000000000 ) ) ;
#2166 = EDGE_CURVE ( 'NONE', #1353, #1097, #814, .T. ) ;
#2167 = SURFACE_STYLE_USAGE ( .BOTH. , #1450 ) ;
#2168 = ORIENTED_EDGE ( 'NONE', *, *, #53, .T. ) ;
#2169 = FACE_OUTER_BOUND ( 'NONE', #2088, .T. ) ;
#2170 = ORIENTED_EDGE ( 'NONE', *, *, #334, .T. ) ;
#2171 = DIRECTION ( 'NONE',  ( -1.000000000000000000, -0.000000000000000000, -0.000000000000000000 ) ) ;
#2172 = DIRECTION ( 'NONE',  ( 0.000000000000000000, 0.000000000000000000, 1.000000000000000000 ) ) ;
#2173 = ADVANCED_FACE ( 'NONE', ( #654 ), #1854, .T. ) ;
#2174 = CARTESIAN_POINT ( 'NONE',  ( 145.0000000000000284, 3.000000000000002665, 45.00000000000000000 ) ) ;
#2175 = CIRCLE ( 'NONE', #1237, 2.649999999999985700 ) ;
#2176 = CARTESIAN_POINT ( 'NONE',  ( -139.9999999999999716, -120.0000000000000142, 50.00000000000000000 ) ) ;
#2177 = EDGE_CURVE ( 'NONE', #324, #1430, #1516, .T. ) ;
#2178 = EDGE_CURVE ( 'NONE', #1293, #1125, #1491, .T. ) ;
#2179 = ORIENTED_EDGE ( 'NONE', *, *, #633, .F. ) ;
#2180 = CARTESIAN_POINT ( 'NONE',  ( 0.000000000000000000, 2.357898499370431722, -2.818925648462311528E-15 ) ) ;
#2181 = EDGE_LOOP ( 'NONE', ( #2019, #225 ) ) ;
#2182 = FACE_OUTER_BOUND ( 'NONE', #647, .T. ) ;
#2183 = CARTESIAN_POINT ( 'NONE',  ( 145.0000000000000284, 2.993649167310367343, 45.00000000000000000 ) ) ;
#2184 = PRESENTATION_LAYER_ASSIGNMENT (  '', '', ( #1506 ) ) ;
#2185 = DIRECTION ( 'NONE',  ( 0.000000000000000000, 0.000000000000000000, 1.000000000000000000 ) ) ;
#2186 = LINE ( 'NONE', #2042, #501 ) ;
#2187 = ITEM_DEFINED_TRANSFORMATION ( 'NONE', 'NONE', #369,  #30 ) ;
#2188 = PRESENTATION_STYLE_ASSIGNMENT (( #2167 ) ) ;
#2189 = AXIS2_PLACEMENT_3D ( 'NONE', #1633, #629, #76 ) ;
#2190 = ORIENTED_EDGE ( 'NONE', *, *, #2208, .T. ) ;
#2191 = DIRECTION ( 'NONE',  ( 0.000000000000000000, -1.000000000000000000, 1.287488025362403787E-15 ) ) ;
#2192 = VERTEX_POINT ( 'NONE', #959 ) ;
#2193 = CYLINDRICAL_SURFACE ( 'NONE', #1599, 2.649999999999985700 ) ;
#2194 = EDGE_CURVE ( 'NONE', #805, #738, #1480, .T. ) ;
#2195 = DIRECTION ( 'NONE',  ( 1.000000000000000000, 0.000000000000000000, 0.000000000000000000 ) ) ;
#2196 = EDGE_CURVE ( 'NONE', #145, #847, #2157, .T. ) ;
#2197 = STYLED_ITEM ( 'NONE', ( #642 ), #1733 ) ;
#2198 = ORIENTED_EDGE ( 'NONE', *, *, #1898, .F. ) ;
#2199 = VECTOR ( 'NONE', #886, 1000.000000000000000 ) ;
#2200 = DIRECTION ( 'NONE',  ( 0.000000000000000000, 0.000000000000000000, 1.000000000000000000 ) ) ;
#2201 = PLANE ( 'NONE',  #203 ) ;
#2202 = CIRCLE ( 'NONE', #2163, 0.1999999999999987899 ) ;
#2203 =( NAMED_UNIT ( * ) SI_UNIT ( $, .STERADIAN. ) SOLID_ANGLE_UNIT ( ) );
#2204 = ADVANCED_FACE ( 'NONE', ( #2169 ), #826, .F. ) ;
#2205 = VERTEX_POINT ( 'NONE', #2003 ) ;
#2206 = CARTESIAN_POINT ( 'NONE',  ( -150.0000000000000000, 0.000000000000000000, 50.00000000000000000 ) ) ;
#2207 = ORIENTED_EDGE ( 'NONE', *, *, #281, .F. ) ;
#2208 = EDGE_CURVE ( 'NONE', #1444, #1316, #2056, .T. ) ;
#2209 = FACE_OUTER_BOUND ( 'NONE', #1763, .T. ) ;
#2210 = DIRECTION ( 'NONE',  ( 0.000000000000000000, 0.000000000000000000, 1.000000000000000000 ) ) ;
#2211 = UNCERTAINTY_MEASURE_WITH_UNIT (LENGTH_MEASURE( 1.000000000000000082E-05 ), #247, 'distance_accuracy_value', 'NONE');
#2212 = EDGE_CURVE ( 'NONE', #1831, #830, #1874, .T. ) ;
#2213 = ORIENTED_EDGE ( 'NONE', *, *, #703, .T. ) ;
#2214 = CARTESIAN_POINT ( 'NONE',  ( 2.500000000000000000, -2.357898499370432166, 3.035766082959412415E-15 ) ) ;
#2215 = CARTESIAN_POINT ( 'NONE',  ( -150.0000000000000000, 0.000000000000000000, 50.00000000000000000 ) ) ;
#2216 = DIRECTION ( 'NONE',  ( 0.000000000000000000, 0.000000000000000000, 1.000000000000000000 ) ) ;
#2217 = ORIENTED_EDGE ( 'NONE', *, *, #767, .T. ) ;
#2218 = VERTEX_POINT ( 'NONE', #1305 ) ;
#2219 = AXIS2_PLACEMENT_3D ( 'NONE', #529, #1727, #1709 ) ;
#2220 = PLANE ( 'NONE',  #1073 ) ;
#2221 = CARTESIAN_POINT ( 'NONE',  ( -145.0000000000000284, -3.358697307418414604E-14, 45.00000000000000000 ) ) ;
#2222 = ORIENTED_EDGE ( 'NONE', *, *, #318, .T. ) ;
#2223 = CARTESIAN_POINT ( 'NONE',  ( -157.0000000000000000, 3.000000000000000000, -56.99999999999997868 ) ) ;
#2224 = AXIS2_PLACEMENT_3D ( 'NONE', #1836, #304, #591 ) ;
#2225 = FILL_AREA_STYLE_COLOUR ( '', #620 ) ;
#2226 = CARTESIAN_POINT ( 'NONE',  ( -145.0000000000000284, 0.000000000000000000, 45.00000000000000000 ) ) ;
#2227 = NEXT_ASSEMBLY_USAGE_OCCURRENCE ( 'NAUO1', ' ', ' ', #822, #453, $ ) ;
#2228 = NEXT_ASSEMBLY_USAGE_OCCURRENCE ( 'NAUO2', ' ', ' ', #822, #1642, $ ) ;
#2229 = NEXT_ASSEMBLY_USAGE_OCCURRENCE ( 'NAUO3', ' ', ' ', #822, #453, $ ) ;
#2230 = NEXT_ASSEMBLY_USAGE_OCCURRENCE ( 'NAUO4', ' ', ' ', #822, #1410, $ ) ;
#2231 = NEXT_ASSEMBLY_USAGE_OCCURRENCE ( 'NAUO5', ' ', ' ', #822, #1410, $ ) ;
#2232 = NEXT_ASSEMBLY_USAGE_OCCURRENCE ( 'NAUO6', ' ', ' ', #822, #1410, $ ) ;
#2233 = NEXT_ASSEMBLY_USAGE_OCCURRENCE ( 'NAUO7', ' ', ' ', #822, #1410, $ ) ;
#2234=COLOUR_RGB('Dark Blue',0.08,0.2,0.34);
#2235=FILL_AREA_STYLE_COLOUR('',#2234);
#2236=FILL_AREA_STYLE('',(#2235));
#2237=SURFACE_STYLE_FILL_AREA(#2236);
#2238=SURFACE_SIDE_STYLE('',(#2237));
#2239=SURFACE_STYLE_USAGE(.BOTH.,#2238);
#2240=PRESENTATION_STYLE_ASSIGNMENT((#2239));
#2241=COLOUR_RGB('Light Blue',0.38,0.62,0.78);
#2242=FILL_AREA_STYLE_COLOUR('',#2241);
#2243=FILL_AREA_STYLE('',(#2242));
#2244=SURFACE_STYLE_FILL_AREA(#2243);
#2245=SURFACE_SIDE_STYLE('',(#2244));
#2246=SURFACE_STYLE_USAGE(.BOTH.,#2245);
#2247=PRESENTATION_STYLE_ASSIGNMENT((#2246));
#2248=COLOUR_RGB('Sky Blue',0.24,0.69,0.87);
#2249=FILL_AREA_STYLE_COLOUR('',#2248);
#2250=FILL_AREA_STYLE('',(#2249));
#2251=SURFACE_STYLE_FILL_AREA(#2250);
#2252=SURFACE_SIDE_STYLE('',(#2251));
#2253=SURFACE_STYLE_USAGE(.BOTH.,#2252);
#2254=PRESENTATION_STYLE_ASSIGNMENT((#2253));
#2255=COLOUR_RGB('Grey',0.48,0.52,0.57);
#2256=FILL_AREA_STYLE_COLOUR('',#2255);
#2257=FILL_AREA_STYLE('',(#2256));
#2258=SURFACE_STYLE_FILL_AREA(#2257);
#2259=SURFACE_SIDE_STYLE('',(#2258));
#2260=SURFACE_STYLE_USAGE(.BOTH.,#2259);
#2261=PRESENTATION_STYLE_ASSIGNMENT((#2260));
#2262=COLOUR_RGB('Black',0.12,0.14,0.17);
#2263=FILL_AREA_STYLE_COLOUR('',#2262);
#2264=FILL_AREA_STYLE('',(#2263));
#2265=SURFACE_STYLE_FILL_AREA(#2264);
#2266=SURFACE_SIDE_STYLE('',(#2265));
#2267=SURFACE_STYLE_USAGE(.BOTH.,#2266);
#2268=PRESENTATION_STYLE_ASSIGNMENT((#2267));
#2269=COLOUR_RGB('Off White',0.89,0.88,0.83);
#2270=FILL_AREA_STYLE_COLOUR('',#2269);
#2271=FILL_AREA_STYLE('',(#2270));
#2272=SURFACE_STYLE_FILL_AREA(#2271);
#2273=SURFACE_SIDE_STYLE('',(#2272));
#2274=SURFACE_STYLE_USAGE(.BOTH.,#2273);
#2275=PRESENTATION_STYLE_ASSIGNMENT((#2274));
ENDSEC;
END-ISO-10303-21;
